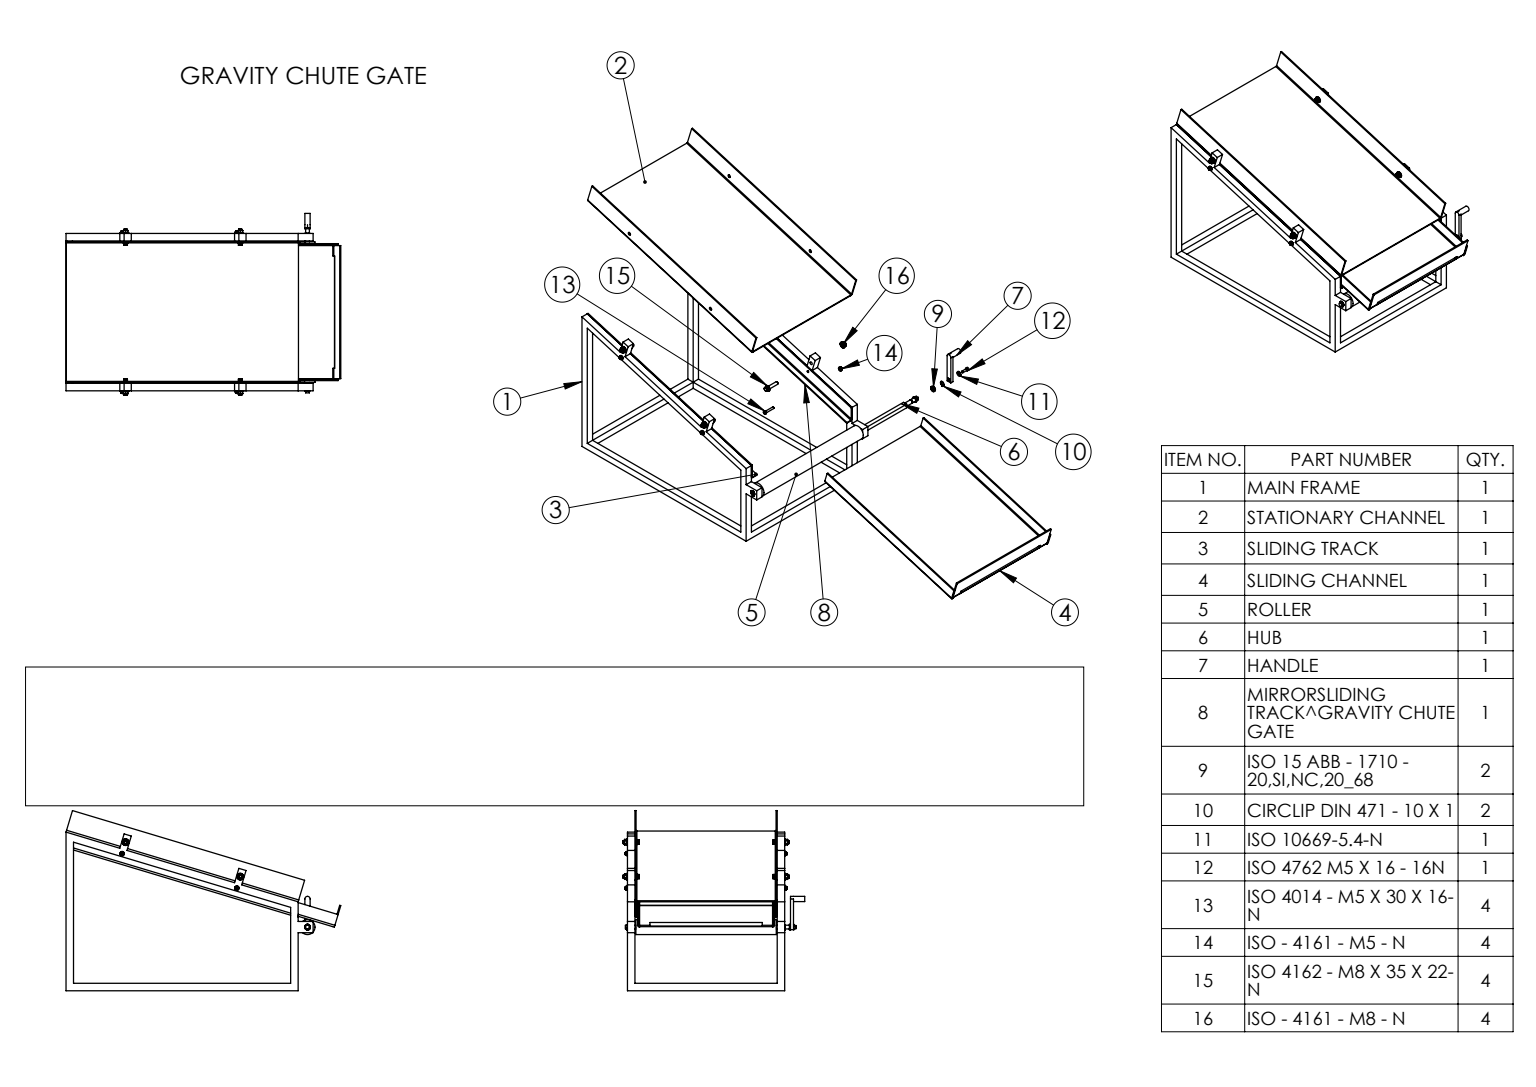
ISO-10303-21;
HEADER;
FILE_DESCRIPTION (('STEP AP214'),
    '1' );
FILE_NAME ('MAS-180',
    '2026-10-27T17:01:19',
    ( '' ),
    ( '' ),
    'SwSTEP 2.0',
    'SolidWorks 2026',
    '' );
FILE_SCHEMA (( 'AUTOMOTIVE_DESIGN' ));
ENDSEC;

DATA;
#1 = AXIS2_PLACEMENT_3D ( 'NONE', #9053, #14371, #13552 ) ;
#2 = DIRECTION ( 'NONE',  ( 1.000000000000000000, 0.000000000000000000, 0.000000000000000000 ) ) ;
#3 = ORIENTED_EDGE ( 'NONE', *, *, #2101, .F. ) ;
#4 = CIRCLE ( 'NONE', #4048, 4.799999999999999822 ) ;
#5 = ORIENTED_EDGE ( 'NONE', *, *, #10243, .F. ) ;
#6 = CARTESIAN_POINT ( 'NONE',  ( 1.058054217398695762, -6.894685612232789751, -0.3576316571898509600 ) ) ;
#7 = EDGE_CURVE ( 'NONE', #11993, #2660, #12348, .T. ) ;
#8 = FACE_OUTER_BOUND ( 'NONE', #13413, .T. ) ;
#9 = CIRCLE ( 'NONE', #4050, 0.7500000000000000000 ) ;
#10 = DIRECTION ( 'NONE',  ( 0.000000000000000000, 0.000000000000000000, -1.000000000000000000 ) ) ;
#11 = FACE_OUTER_BOUND ( 'NONE', #11887, .T. ) ;
#12 = ORIENTED_EDGE ( 'NONE', *, *, #9612, .F. ) ;
#13 =( GEOMETRIC_REPRESENTATION_CONTEXT ( 3 ) GLOBAL_UNCERTAINTY_ASSIGNED_CONTEXT ( ( #9752 ) ) GLOBAL_UNIT_ASSIGNED_CONTEXT ( ( #1212, #12871, #12805 ) ) REPRESENTATION_CONTEXT ( 'NONE', 'WORKASPACE' ) );
#14 = CARTESIAN_POINT ( 'NONE',  ( 640.0000000000000000, 160.0000000000000284, -222.5000000000000000 ) ) ;
#15 = EDGE_LOOP ( 'NONE', ( #6802, #6787, #9525 ) ) ;
#16 = ORIENTED_EDGE ( 'NONE', *, *, #2742, .F. ) ;
#17 = CARTESIAN_POINT ( 'NONE',  ( 6.212060063025091061, 2.039954613760103896, -5.000000000000000000 ) ) ;
#18 = EDGE_LOOP ( 'NONE', ( #9492, #7040, #7243, #2975 ) ) ;
#19 = TOROIDAL_SURFACE ( 'NONE', #6418, 2.700000000000000622, 0.2000000000000000111 ) ;
#20 = DIRECTION ( 'NONE',  ( 0.3420201433256622736, 1.150791560227853228E-16, 0.9396926207859106484 ) ) ;
#21 = CARTESIAN_POINT ( 'NONE',  ( 148.9991633467111569, 386.6211705227183870, -190.0000000000000000 ) ) ;
#22 = B_SPLINE_CURVE_WITH_KNOTS ( 'NONE', 3,
 ( #2566, #497, #13861, #11570, #12830, #4870, #11639, #4939 ),
 .UNSPECIFIED., .F., .F.,
 ( 4, 2, 2, 4 ),
 ( 0.002921158011986709890, 0.003648658599403064012, 0.004376159186819418567, 0.005831160361652128546 ),
 .UNSPECIFIED. ) ;
#23 = ORIENTED_EDGE ( 'NONE', *, *, #607, .T. ) ;
#24 = CARTESIAN_POINT ( 'NONE',  ( 6.244297270354683960, 1.800816419761795034E-11, 5.105276777067893512 ) ) ;
#25 = EDGE_CURVE ( 'NONE', #3163, #4002, #6451, .T. ) ;
#26 = DIRECTION ( 'NONE',  ( 0.000000000000000000, 0.000000000000000000, 1.000000000000000000 ) ) ;
#27 = FACE_OUTER_BOUND ( 'NONE', #636, .T. ) ;
#28 =( NAMED_UNIT ( * ) SI_UNIT ( $, .STERADIAN. ) SOLID_ANGLE_UNIT ( ) );
#29 = AXIS2_PLACEMENT_3D ( 'NONE', #668, #3321, #5190 ) ;
#30 = VERTEX_POINT ( 'NONE', #596 ) ;
#31 = EDGE_CURVE ( 'NONE', #4518, #4002, #1965, .T. ) ;
#32 = CARTESIAN_POINT ( 'NONE',  ( 0.000000000000000000, 0.000000000000000000, -25.03750572909317285 ) ) ;
#33 = ORIENTED_EDGE ( 'NONE', *, *, #12524, .T. ) ;
#34 = EDGE_CURVE ( 'NONE', #1936, #10044, #4903, .T. ) ;
#35 = AXIS2_PLACEMENT_3D ( 'NONE', #1338, #10342, #11594 ) ;
#36 = ORIENTED_EDGE ( 'NONE', *, *, #12069, .F. ) ;
#37 = CARTESIAN_POINT ( 'NONE',  ( 0.000000000000000000, 0.000000000000000000, -187.5000000000000000 ) ) ;
#38 = ADVANCED_FACE ( 'NONE', ( #6155 ), #1724, .F. ) ;
#39 = DIRECTION ( 'NONE',  ( 1.000000000000000000, 0.000000000000000000, 0.000000000000000000 ) ) ;
#40 = VECTOR ( 'NONE', #12593, 1000.000000000000000 ) ;
#41 = CARTESIAN_POINT ( 'NONE',  ( 164.3243839102495656, 402.9042173714779551, -210.0000000000000000 ) ) ;
#42 = CARTESIAN_POINT ( 'NONE',  ( 0.000000000000000000, 0.000000000000000000, 0.000000000000000000 ) ) ;
#43 = DIRECTION ( 'NONE',  ( 0.000000000000000000, 0.000000000000000000, -1.000000000000000000 ) ) ;
#44 = DIRECTION ( 'NONE',  ( 1.000000000000000000, 0.000000000000000000, -0.000000000000000000 ) ) ;
#45 = CARTESIAN_POINT ( 'NONE',  ( 702.5260191523640287, 164.1854586329053518, -177.6000000000005059 ) ) ;
#46 = ORIENTED_EDGE ( 'NONE', *, *, #6815, .F. ) ;
#47 = CYLINDRICAL_SURFACE ( 'NONE', #4191, 4.000000000000000000 ) ;
#48 = CARTESIAN_POINT ( 'NONE',  ( 6.527192678185238961, -5.883244248022514888, -3.079566767404799650E-14 ) ) ;
#49 = APPLICATION_PROTOCOL_DEFINITION ( 'draft international standard', 'automotive_design', 1998, #11586 ) ;
#50 = EDGE_LOOP ( 'NONE', ( #5774, #9979, #12011, #287 ) ) ;
#51=STYLED_ITEM('',(#14681),#12291);
#52 = ADVANCED_FACE ( 'NONE', ( #11739, #7114 ), #5117, .T. ) ;
#53 = CARTESIAN_POINT ( 'NONE',  ( 629.0000000000000000, 166.0000000000000284, -187.5000000000000000 ) ) ;
#54 = VERTEX_POINT ( 'NONE', #6074 ) ;
#55 = EDGE_LOOP ( 'NONE', ( #10980, #1481, #10748, #12698 ) ) ;
#56 = CARTESIAN_POINT ( 'NONE',  ( -20.63749999999999574, 0.000000000000000000, -6.975000000000000533 ) ) ;
#57 = CARTESIAN_POINT ( 'NONE',  ( -6.500000000000000000, 3.752776749732564809, -6.064240316920399110 ) ) ;
#58 = EDGE_CURVE ( 'NONE', #5396, #13410, #5058, .T. ) ;
#59 = FACE_OUTER_BOUND ( 'NONE', #3908, .T. ) ;
#60 = PLANE ( 'NONE',  #2621 ) ;
#61 = DIRECTION ( 'NONE',  ( 0.000000000000000000, 0.000000000000000000, 1.000000000000000000 ) ) ;
#62 = EDGE_LOOP ( 'NONE', ( #9424, #13653, #13087, #10601 ) ) ;
#63 = CARTESIAN_POINT ( 'NONE',  ( 6.244297270354684848, -1.799661607120071246E-11, -5.105276777067894400 ) ) ;
#64 = DIRECTION ( 'NONE',  ( 0.000000000000000000, 0.000000000000000000, 1.000000000000000000 ) ) ;
#65 = DIRECTION ( 'NONE',  ( 1.000000000000000000, 0.000000000000000000, 0.000000000000000000 ) ) ;
#66 = DIRECTION ( 'NONE',  ( 0.000000000000000000, 0.000000000000000000, 1.000000000000000000 ) ) ;
#67 = ORIENTED_EDGE ( 'NONE', *, *, #6101, .T. ) ;
#68 = ORIENTED_EDGE ( 'NONE', *, *, #2122, .F. ) ;
#69 = CARTESIAN_POINT ( 'NONE',  ( -3.511755186886750479, 2.826662030176366081, -3.597382984111578086 ) ) ;
#70 = PLANE ( 'NONE',  #7516 ) ;
#71 = CARTESIAN_POINT ( 'NONE',  ( -4.197393957002303999, 0.4069871074557429025, -3.503767560748926257 ) ) ;
#72 = VERTEX_POINT ( 'NONE', #2614 ) ;
#73 = B_SPLINE_CURVE_WITH_KNOTS ( 'NONE', 3,
 ( #5275, #111, #2574, #7961, #9298 ),
 .UNSPECIFIED., .F., .F.,
 ( 4, 1, 4 ),
 ( 0.000000000000000000, 0.002886751345948128985, 0.005773502691896257970 ),
 .UNSPECIFIED. ) ;
#74 = EDGE_LOOP ( 'NONE', ( #5773, #12707 ) ) ;
#75 = CARTESIAN_POINT ( 'NONE',  ( 609.6905198467529772, 186.4571330906553044, -187.4188186979287423 ) ) ;
#76 = CARTESIAN_POINT ( 'NONE',  ( 451.6722694765949768, 316.6998517015743460, -210.0000000000000000 ) ) ;
#77 = EDGE_CURVE ( 'NONE', #2441, #3014, #1734, .T. ) ;
#78 = DIRECTION ( 'NONE',  ( 0.000000000000000000, 0.000000000000000000, -1.000000000000000000 ) ) ;
#79 = CARTESIAN_POINT ( 'NONE',  ( 650.0000000000000000, 175.0000000000000568, 190.0000000000000000 ) ) ;
#80 = CARTESIAN_POINT ( 'NONE',  ( 459.7035746174795463, 294.6698471414878782, 210.0000000000000000 ) ) ;
#81 = ORIENTED_EDGE ( 'NONE', *, *, #14582, .T. ) ;
#82 = DIRECTION ( 'NONE',  ( 1.000000000000000000, 0.000000000000000000, 0.000000000000000000 ) ) ;
#83 = ORIENTED_EDGE ( 'NONE', *, *, #7565, .F. ) ;
#84 = ORIENTED_EDGE ( 'NONE', *, *, #4575, .F. ) ;
#85 = CARTESIAN_POINT ( 'NONE',  ( 642.5000000000001137, 160.0000000000000284, -207.0000000000000000 ) ) ;
#86 = ORIENTED_EDGE ( 'NONE', *, *, #13517, .T. ) ;
#87 = ADVANCED_FACE ( 'NONE', ( #9552, #4013, #2686 ), #14052, .T. ) ;
#88 = EDGE_CURVE ( 'NONE', #5056, #3419, #11622, .T. ) ;
#89 = CARTESIAN_POINT ( 'NONE',  ( 0.000000000000000000, 0.000000000000000000, -7.381345277524544279 ) ) ;
#90 = DIRECTION ( 'NONE',  ( 1.000000000000000000, 0.000000000000000000, 0.000000000000000000 ) ) ;
#91 = ORIENTED_EDGE ( 'NONE', *, *, #14281, .F. ) ;
#92 = CARTESIAN_POINT ( 'NONE',  ( 2.500000000000000888, 3.061616997868384127E-16, -4.974599999999998801 ) ) ;
#93 = DIRECTION ( 'NONE',  ( 0.9578262852211525402, -0.2873478855663419429, -0.000000000000000000 ) ) ;
#94 = DIRECTION ( 'NONE',  ( 1.000000000000000000, 0.000000000000000000, 0.000000000000000000 ) ) ;
#95 = SURFACE_STYLE_USAGE ( .BOTH. , #11266 ) ;
#96 = SHAPE_REPRESENTATION_RELATIONSHIP ( 'NONE' , 'NONE' ,  #14430, #6538 ) ;
#97 = ORIENTED_EDGE ( 'NONE', *, *, #10462, .F. ) ;
#98 = PLANE ( 'NONE',  #9893 ) ;
#99 = EDGE_LOOP ( 'NONE', ( #7071, #6114, #7487, #2779 ) ) ;
#100 = EDGE_LOOP ( 'NONE', ( #955, #2493 ) ) ;
#101 = DIRECTION ( 'NONE',  ( 0.000000000000000000, 0.000000000000000000, 1.000000000000000000 ) ) ;
#102 = ADVANCED_FACE ( 'NONE', ( #9327 ), #3935, .F. ) ;
#103 = CARTESIAN_POINT ( 'NONE',  ( 642.4999005938085475, 159.0059381730093548, -210.0000000000000284 ) ) ;
#104 = CARTESIAN_POINT ( 'NONE',  ( 642.5000000000001137, 160.0000000000000284, 210.0000119999999981 ) ) ;
#105 = LINE ( 'NONE', #11206, #8037 ) ;
#106 = EDGE_CURVE ( 'NONE', #2067, #2328, #1941, .T. ) ;
#107 = CARTESIAN_POINT ( 'NONE',  ( 0.3572655899081578768, -4.618802153516999631, -3.329030144205522754E-16 ) ) ;
#108 = CARTESIAN_POINT ( 'NONE',  ( 610.0000000000000000, 227.4403065089097993, 184.7999999999999829 ) ) ;
#109 = DIRECTION ( 'NONE',  ( 0.000000000000000000, 0.000000000000000000, 1.000000000000000000 ) ) ;
#110 = EDGE_LOOP ( 'NONE', ( #11251, #9027, #7663, #8176 ) ) ;
#111 = CARTESIAN_POINT ( 'NONE',  ( 6.196878017913832970, -3.367876570272823500, -4.166666666666666963 ) ) ;
#112 = CARTESIAN_POINT ( 'NONE',  ( 0.000000000000000000, 0.000000000000000000, -4.974599999999998801 ) ) ;
#113 = CARTESIAN_POINT ( 'NONE',  ( 6.403457969954073015, -5.776886471390939803, 5.182398524903814613E-16 ) ) ;
#114 = CONTEXT_DEPENDENT_SHAPE_REPRESENTATION ( #6028, #6295 ) ;
#115 = ORIENTED_EDGE ( 'NONE', *, *, #8446, .T. ) ;
#116 = CARTESIAN_POINT ( 'NONE',  ( 145.1678582058265476, 408.6511750828048548, -190.0000000000000000 ) ) ;
#117 = ORIENTED_EDGE ( 'NONE', *, *, #9862, .T. ) ;
#118 = ORIENTED_EDGE ( 'NONE', *, *, #8596, .T. ) ;
#119 = SURFACE_STYLE_USAGE ( .BOTH. , #3632 ) ;
#120 = DIRECTION ( 'NONE',  ( -1.673149720584257832E-16, 4.625616335171366110E-15, 1.000000000000000000 ) ) ;
#121 = EDGE_CURVE ( 'NONE', #14270, #6163, #532, .T. ) ;
#122 = CARTESIAN_POINT ( 'NONE',  ( 6.534838248920896930, -2.951765777552407766, 5.112608298763836601 ) ) ;
#123 = EDGE_CURVE ( 'NONE', #7138, #2816, #1501, .T. ) ;
#124 = PRODUCT ( 'plain washer 10669 type nl_iso_ISO 10669-5.4-N', 'plain washer 10669 type nl_iso_ISO 10669-5.4-N', '', ( #6717 ) ) ;
#125 = CARTESIAN_POINT ( 'NONE',  ( 716.7018481736364492, 193.3416907550361827, -179.8000000000001535 ) ) ;
#126 = EDGE_CURVE ( 'NONE', #13510, #3531, #3853, .T. ) ;
#127 = UNCERTAINTY_MEASURE_WITH_UNIT (LENGTH_MEASURE( 1.000000000000000082E-05 ), #3308, 'distance_accuracy_value', 'NONE');
#128 = CARTESIAN_POINT ( 'NONE',  ( 630.0000000000000000, 160.0000000000000284, 215.5000000000000000 ) ) ;
#129 = ORIENTED_EDGE ( 'NONE', *, *, #11764, .F. ) ;
#130 = EDGE_CURVE ( 'NONE', #2847, #2989, #365, .T. ) ;
#131 = DIRECTION ( 'NONE',  ( 0.000000000000000000, 0.000000000000000000, 1.000000000000000000 ) ) ;
#132 = CARTESIAN_POINT ( 'NONE',  ( 610.0000000000000000, 0.000000000000000000, -210.0000000000000000 ) ) ;
#133 = SURFACE_STYLE_FILL_AREA ( #3350 ) ;
#134 = CARTESIAN_POINT ( 'NONE',  ( 650.0000000000000000, 0.000000000000000000, 0.000000000000000000 ) ) ;
#135 = ORIENTED_EDGE ( 'NONE', *, *, #9646, .T. ) ;
#136 = ORIENTED_EDGE ( 'NONE', *, *, #1223, .F. ) ;
#137 = CARTESIAN_POINT ( 'NONE',  ( 641.5533979126569193, 156.2228576472182624, 210.0000119999999981 ) ) ;
#138 = DIRECTION ( 'NONE',  ( -1.000000000000000000, 0.000000000000000000, 0.000000000000000000 ) ) ;
#139 = LINE ( 'NONE', #7921, #12453 ) ;
#140 = CARTESIAN_POINT ( 'NONE',  ( 9.498873539028489220E-16, -10.00000000000000000, 210.0000000000000000 ) ) ;
#141 = EDGE_CURVE ( 'NONE', #2225, #13547, #11826, .T. ) ;
#143 = ORIENTED_EDGE ( 'NONE', *, *, #1858, .T. ) ;
#142 = CIRCLE ( 'NONE', #4214, 5.000000000000004441 ) ;
#144 = VECTOR ( 'NONE', #10565, 1000.000000000000000 ) ;
#145 = VERTEX_POINT ( 'NONE', #14118 ) ;
#146 = DIRECTION ( 'NONE',  ( 0.000000000000000000, 0.000000000000000000, -1.000000000000000000 ) ) ;
#147 = DIRECTION ( 'NONE',  ( 0.000000000000000000, 0.000000000000000000, 1.000000000000000000 ) ) ;
#148 = FACE_BOUND ( 'NONE', #8389, .T. ) ;
#149 = DIRECTION ( 'NONE',  ( 0.000000000000000000, 1.000000000000000000, -4.159212477520619976E-15 ) ) ;
#150 = CARTESIAN_POINT ( 'NONE',  ( 142.4540310085880606, 355.9707293956415697, 187.0000000000000000 ) ) ;
#151 = VERTEX_POINT ( 'NONE', #13018 ) ;
#152 = CYLINDRICAL_SURFACE ( 'NONE', #12239, 4.000000000000000000 ) ;
#153 = EDGE_LOOP ( 'NONE', ( #10187, #6954 ) ) ;
#154 = ORIENTED_EDGE ( 'NONE', *, *, #12359, .F. ) ;
#155 = CARTESIAN_POINT ( 'NONE',  ( -6.259644161404860030E-16, -4.618802153517027165, -5.000000000000000000 ) ) ;
#156 = VECTOR ( 'NONE', #9588, 1000.000000000000000 ) ;
#157 = EDGE_CURVE ( 'NONE', #12209, #11318, #10435, .T. ) ;
#158 = VECTOR ( 'NONE', #9040, 1000.000000000000000 ) ;
#159 = PRODUCT_DEFINITION_SHAPE ( 'NONE', 'NONE',  #14640 ) ;
#160 = ADVANCED_FACE ( 'NONE', ( #9907 ), #3261, .F. ) ;
#161 = CARTESIAN_POINT ( 'NONE',  ( 112.3905262037967248, 374.6350873459896320, 182.7999999999994714 ) ) ;
#162 =( REPRESENTATION_RELATIONSHIP ('NONE','NONE', #2822, #5462 ) REPRESENTATION_RELATIONSHIP_WITH_TRANSFORMATION ( #13326 )SHAPE_REPRESENTATION_RELATIONSHIP( ) );
#163 = DIRECTION ( 'NONE',  ( 1.000000000000000000, 0.000000000000000000, 0.000000000000000000 ) ) ;
#164 = ORIENTED_EDGE ( 'NONE', *, *, #10968, .F. ) ;
#165 = CARTESIAN_POINT ( 'NONE',  ( 459.3348797583642522, 272.6398425814014104, -210.0000000000000000 ) ) ;
#166 = FACE_OUTER_BOUND ( 'NONE', #2918, .T. ) ;
#167 = AXIS2_PLACEMENT_3D ( 'NONE', #3930, #8417, #10718 ) ;
#168 = AXIS2_PLACEMENT_3D ( 'NONE', #10064, #3978, #5431 ) ;
#169 = CARTESIAN_POINT ( 'NONE',  ( 1.500000000000001332, 0.000000000000000000, 0.000000000000000000 ) ) ;
#170 = CARTESIAN_POINT ( 'NONE',  ( 0.6507732100473444525, -4.243078065514795050, -0.2236248678334952777 ) ) ;
#171 = ORIENTED_EDGE ( 'NONE', *, *, #13700, .T. ) ;
#172 = DIRECTION ( 'NONE',  ( 3.340694023494469140E-16, -4.069768234201303760E-15, -1.000000000000000000 ) ) ;
#173 = VERTEX_POINT ( 'NONE', #3127 ) ;
#174 = ORIENTED_EDGE ( 'NONE', *, *, #7655, .T. ) ;
#175 = LINE ( 'NONE', #4721, #7503 ) ;
#176 = VECTOR ( 'NONE', #3313, 1000.000000000000000 ) ;
#177 = MECHANICAL_DESIGN_GEOMETRIC_PRESENTATION_REPRESENTATION (  '', ( #1004 ), #8687 ) ;
#178 = DIRECTION ( 'NONE',  ( 0.000000000000000000, 0.000000000000000000, -1.000000000000000000 ) ) ;
#179 = DIRECTION ( 'NONE',  ( -1.000000000000000000, -0.000000000000000000, -0.000000000000000000 ) ) ;
#180 = ORIENTED_EDGE ( 'NONE', *, *, #12151, .F. ) ;
#181 = DIRECTION ( 'NONE',  ( 1.000000000000000000, 0.000000000000000000, 0.000000000000000000 ) ) ;
#182 = CIRCLE ( 'NONE', #10114, 0.2000000000000000944 ) ;
#183 = CARTESIAN_POINT ( 'NONE',  ( 610.0421465541240877, 190.7920056415575516, -186.9999999999999432 ) ) ;
#184 = CARTESIAN_POINT ( 'NONE',  ( -6.826425371444817536, 2.641426549045769345, -6.344843397090116355 ) ) ;
#185 = PLANE ( 'NONE',  #4357 ) ;
#186 = EDGE_CURVE ( 'NONE', #3815, #10556, #4083, .T. ) ;
#187 = ORIENTED_EDGE ( 'NONE', *, *, #791, .F. ) ;
#188 = VECTOR ( 'NONE', #2606, 1000.000000000000000 ) ;
#189 = AXIS2_PLACEMENT_3D ( 'NONE', #8607, #13111, #14291 ) ;
#190 = FACE_OUTER_BOUND ( 'NONE', #11579, .T. ) ;
#191 = DIRECTION ( 'NONE',  ( 1.000000000000000000, 0.000000000000000000, 0.000000000000000000 ) ) ;
#192 = LINE ( 'NONE', #8454, #3753 ) ;
#193 = EDGE_LOOP ( 'NONE', ( #2834, #237, #12964, #6241 ) ) ;
#194 = VECTOR ( 'NONE', #6776, 1000.000000000000000 ) ;
#195 = CARTESIAN_POINT ( 'NONE',  ( 6.327640840229819652, -2.033197012992983943, 4.999999999998298250 ) ) ;
#196 = ORIENTED_EDGE ( 'NONE', *, *, #8935, .F. ) ;
#197 = VERTEX_POINT ( 'NONE', #7549 ) ;
#198 = DIRECTION ( 'NONE',  ( -1.000000000000000000, 0.000000000000000000, 0.000000000000000000 ) ) ;
#199 = CARTESIAN_POINT ( 'NONE',  ( 726.1975094929949819, 167.5243180396262801, -149.9999999999986358 ) ) ;
#200 = VECTOR ( 'NONE', #9426, 1000.000000000000000 ) ;
#201 = CARTESIAN_POINT ( 'NONE',  ( 0.000000000000000000, 0.000000000000000000, 6.250000000000000000 ) ) ;
#202 = VECTOR ( 'NONE', #5695, 1000.000000000000000 ) ;
#203 = AXIS2_PLACEMENT_3D ( 'NONE', #4127, #790, #8616 ) ;
#204 = CARTESIAN_POINT ( 'NONE',  ( 6.269955739554010421, 4.268932597852939104, -6.443844059477442876 ) ) ;
#205 = LINE ( 'NONE', #12625, #7486 ) ;
#206 = ADVANCED_FACE ( 'NONE', ( #6452 ), #11002, .F. ) ;
#207 = ORIENTED_EDGE ( 'NONE', *, *, #12524, .F. ) ;
#208 = CIRCLE ( 'NONE', #11778, 8.542937654374687995 ) ;
#209 = FACE_OUTER_BOUND ( 'NONE', #12548, .T. ) ;
#210 = DIRECTION ( 'NONE',  ( 0.000000000000000000, 0.000000000000000000, 1.000000000000000000 ) ) ;
#211 = EDGE_CURVE ( 'NONE', #1708, #13374, #7694, .T. ) ;
#212 = VECTOR ( 'NONE', #12362, 1000.000000000000000 ) ;
#213 = DIRECTION ( 'NONE',  ( 0.000000000000000000, -0.000000000000000000, -1.000000000000000000 ) ) ;
#214 = VERTEX_POINT ( 'NONE', #14200 ) ;
#215 = ORIENTED_EDGE ( 'NONE', *, *, #1697, .T. ) ;
#216 = CARTESIAN_POINT ( 'NONE',  ( 640.9975013179864618, 155.3908996001881064, 210.0000119999999981 ) ) ;
#217 = CARTESIAN_POINT ( 'NONE',  ( 145.1678582058265192, 408.6511750828049117, 210.0000000000000000 ) ) ;
#218 = EDGE_CURVE ( 'NONE', #4236, #7201, #9506, .T. ) ;
#219 = CARTESIAN_POINT ( 'NONE',  ( 6.390820841722129941, 2.823237767533145703, 5.110008744785254464 ) ) ;
#220 = CIRCLE ( 'NONE', #10375, 2.199999999999988187 ) ;
#221 = AXIS2_PLACEMENT_3D ( 'NONE', #1029, #9011, #10110 ) ;
#222 = EDGE_CURVE ( 'NONE', #5688, #13812, #7865, .T. ) ;
#223 = CIRCLE ( 'NONE', #9439, 5.000000000000000000 ) ;
#224 = ORIENTED_EDGE ( 'NONE', *, *, #3254, .F. ) ;
#225 = VECTOR ( 'NONE', #9137, 1000.000000000000114 ) ;
#226 = ORIENTED_EDGE ( 'NONE', *, *, #14281, .T. ) ;
#227 = DIRECTION ( 'NONE',  ( 0.000000000000000000, 0.000000000000000000, -1.000000000000000000 ) ) ;
#228 = CARTESIAN_POINT ( 'NONE',  ( 2.263183130831067924, -6.566419505188284766, -6.208110906918261840 ) ) ;
#229 = LINE ( 'NONE', #12418, #8916 ) ;
#230 = DIRECTION ( 'NONE',  ( -1.000000000000000000, 0.000000000000000000, 0.000000000000000000 ) ) ;
#231 = CARTESIAN_POINT ( 'NONE',  ( 635.0000000000000000, 160.0000000000000284, 215.5000000000000000 ) ) ;
#232 = SURFACE_SIDE_STYLE ('',( #9558 ) ) ;
#233 = VECTOR ( 'NONE', #11079, 1000.000000000000000 ) ;
#234 = ORIENTED_EDGE ( 'NONE', *, *, #11746, .T. ) ;
#235 = AXIS2_PLACEMENT_3D ( 'NONE', #506, #13872, #10410 ) ;
#236 = DIRECTION ( 'NONE',  ( 0.000000000000000000, 0.000000000000000000, 1.000000000000000000 ) ) ;
#237 = ORIENTED_EDGE ( 'NONE', *, *, #8274, .T. ) ;
#238 = VERTEX_POINT ( 'NONE', #752 ) ;
#239 = LINE ( 'NONE', #9271, #6395 ) ;
#240 = EDGE_CURVE ( 'NONE', #4614, #6705, #3374, .T. ) ;
#241 = VECTOR ( 'NONE', #10180, 1000.000000000000000 ) ;
#242 = EDGE_CURVE ( 'NONE', #7278, #11617, #2972, .T. ) ;
#243 = ADVANCED_FACE ( 'NONE', ( #12113 ), #8583, .F. ) ;
#244 = DIRECTION ( 'NONE',  ( 0.9578262852211513190, -0.2873478855663453846, 0.000000000000000000 ) ) ;
#245 = CIRCLE ( 'NONE', #8768, 4.199999999999926459 ) ;
#246 = AXIS2_PLACEMENT_3D ( 'NONE', #1497, #5996, #10494 ) ;
#247 = LINE ( 'NONE', #13705, #494 ) ;
#248 = VERTEX_POINT ( 'NONE', #7468 ) ;
#249 = DIRECTION ( 'NONE',  ( 0.9578262852211507639, -0.2873478855663477716, 0.000000000000000000 ) ) ;
#250 = CARTESIAN_POINT ( 'NONE',  ( 153.1991633467111456, 386.6211705227183870, -210.0000000000000000 ) ) ;
#251 = CARTESIAN_POINT ( 'NONE',  ( 627.2408731339806991, 284.9098836221797342, 190.0000000000001990 ) ) ;
#252 = PLANE ( 'NONE',  #3852 ) ;
#253 = ORIENTED_EDGE ( 'NONE', *, *, #3737, .F. ) ;
#254 = CARTESIAN_POINT ( 'NONE',  ( 10.00000000000000000, 0.000000000000000000, 210.0000000000000000 ) ) ;
#255 = ORIENTED_EDGE ( 'NONE', *, *, #504, .F. ) ;
#256 = VECTOR ( 'NONE', #3741, 1000.000000000000000 ) ;
#257 = ORIENTED_EDGE ( 'NONE', *, *, #4905, .T. ) ;
#258 = CARTESIAN_POINT ( 'NONE',  ( 10.00000000000000000, 386.5596934910894902, -190.0000000000000000 ) ) ;
#259 = COLOUR_RGB ( '',1.000000000000000000, 0.9490196078431372140, 0.9098039215686274384 ) ;
#260 =( BOUNDED_SURFACE ( )  B_SPLINE_SURFACE ( 3, 2, ( 
 ( #2546, #4855, #7134 ),
 ( #13843, #1521, #11762 ),
 ( #3742, #1668, #2637 ),
 ( #552, #8754, #12960 ),
 ( #1882, #8671, #14357 ),
 ( #14286, #6532, #7425 ),
 ( #11025, #772, #8601 ),
 ( #4037, #14440, #13175 ) ),
 .UNSPECIFIED., .F., .F., .F. ) 
 B_SPLINE_SURFACE_WITH_KNOTS ( ( 4, 2, 2, 4 ),
 ( 3, 3 ),
 ( 0.03170918191602133812, 0.03570420671717101924, 0.03770171911774586326, 0.03969923151832070729 ),
 ( 0.000000000000000000, 1.000000000000000000 ),
 .UNSPECIFIED. ) 
 GEOMETRIC_REPRESENTATION_ITEM ( )  RATIONAL_B_SPLINE_SURFACE ( (
 ( 1.000000000000000000, 0.8047781070930550840, 1.000000000000000000),
 ( 1.000000000000000000, 0.8123787894255611874, 1.000000000000000000),
 ( 1.000000000000000000, 0.8190667557154468481, 1.000000000000000000),
 ( 1.000000000000000000, 0.8191933945820784047, 1.000000000000000000),
 ( 1.000000000000000000, 0.8176087340369108114, 1.000000000000000000),
 ( 1.000000000000000000, 0.8122956952719621038, 1.000000000000000000),
 ( 1.000000000000000000, 0.8086308540103167575, 1.000000000000000000),
 ( 1.000000000000000000, 0.8047712493762134711, 1.000000000000000000) ) ) 
 REPRESENTATION_ITEM ( '' )  SURFACE ( )  );
#261 = LINE ( 'NONE', #1530, #10839 ) ;
#262 = DIRECTION ( 'NONE',  ( -0.000000000000000000, -0.000000000000000000, -1.000000000000000000 ) ) ;
#263 = VECTOR ( 'NONE', #2526, 1000.000000000000000 ) ;
#264 = VERTEX_POINT ( 'NONE', #11962 ) ;
#265 = CARTESIAN_POINT ( 'NONE',  ( 459.7035746174795463, 294.6698471414878782, -210.0000000000000000 ) ) ;
#266 = FACE_OUTER_BOUND ( 'NONE', #13109, .T. ) ;
#267 = CARTESIAN_POINT ( 'NONE',  ( 635.0000000000000000, 160.0000000000000284, 211.0000000000000000 ) ) ;
#268 = CARTESIAN_POINT ( 'NONE',  ( 610.0000000000001137, 185.6790804732684137, 184.8000000000000682 ) ) ;
#269 = ORIENTED_EDGE ( 'NONE', *, *, #1906, .F. ) ;
#270 = PRODUCT_DEFINITION_FORMATION_WITH_SPECIFIED_SOURCE ( 'ANY', '', #8554, .NOT_KNOWN. ) ;
#271 = CARTESIAN_POINT ( 'NONE',  ( 21.00000000000000355, 0.000000000000000000, 0.000000000000000000 ) ) ;
#272 = CARTESIAN_POINT ( 'NONE',  ( 6.355827204229361982, 5.411702751981842141, -0.8440485055075606091 ) ) ;
#273 = CONTEXT_DEPENDENT_SHAPE_REPRESENTATION ( #1310, #11832 ) ;
#274 = ORIENTED_EDGE ( 'NONE', *, *, #3153, .F. ) ;
#275 = CARTESIAN_POINT ( 'NONE',  ( 0.000000000000000000, 0.000000000000000000, 0.000000000000000000 ) ) ;
#276 = ORIENTED_EDGE ( 'NONE', *, *, #2072, .F. ) ;
#277 = EDGE_LOOP ( 'NONE', ( #11682, #4913 ) ) ;
#278 = CARTESIAN_POINT ( 'NONE',  ( 4.000000000000000000, -2.309401076758514915, -3.433295621305383349 ) ) ;
#279 = CYLINDRICAL_SURFACE ( 'NONE', #8252, 4.799999999999999822 ) ;
#280 = LINE ( 'NONE', #3777, #11997 ) ;
#281 = EDGE_CURVE ( 'NONE', #5961, #525, #3049, .T. ) ;
#282 = ADVANCED_FACE ( 'NONE', ( #6369 ), #14593, .F. ) ;
#283 = CARTESIAN_POINT ( 'NONE',  ( 112.9652219749295341, 376.5507399164317803, -190.0000000000000000 ) ) ;
#284 = UNCERTAINTY_MEASURE_WITH_UNIT (LENGTH_MEASURE( 1.000000000000000082E-05 ), #8450, 'distance_accuracy_value', 'NONE');
#285 = VECTOR ( 'NONE', #13609, 1000.000000000000000 ) ;
#286 = LINE ( 'NONE', #5042, #1068 ) ;
#287 = ORIENTED_EDGE ( 'NONE', *, *, #8174, .T. ) ;
#288 = DIRECTION ( 'NONE',  ( -0.2873478855663281206, -0.9578262852211566480, -1.261617073437843370E-13 ) ) ;
#289 = LINE ( 'NONE', #6055, #6795 ) ;
#290 = DIRECTION ( 'NONE',  ( 1.000000000000000000, 0.000000000000000000, 0.000000000000000000 ) ) ;
#291 = LINE ( 'NONE', #8346, #11794 ) ;
#292 = ORIENTED_EDGE ( 'NONE', *, *, #6303, .T. ) ;
#293 = VERTEX_POINT ( 'NONE', #4374 ) ;
#294 = FACE_OUTER_BOUND ( 'NONE', #6811, .T. ) ;
#295 = CARTESIAN_POINT ( 'NONE',  ( 3.500000000000000000, 2.309401076758500704, -4.000000000000000000 ) ) ;
#296 = CARTESIAN_POINT ( 'NONE',  ( 6.095473853218515536, 3.806361898857873793, 3.407187799183811983 ) ) ;
#297 = EDGE_CURVE ( 'NONE', #14514, #7459, #997, .T. ) ;
#298 = ORIENTED_EDGE ( 'NONE', *, *, #11153, .T. ) ;
#299 = VERTEX_POINT ( 'NONE', #5768 ) ;
#300 = CARTESIAN_POINT ( 'NONE',  ( 650.0000000000000000, 175.0000000000000568, 210.0000000000000000 ) ) ;
#301 = FACE_OUTER_BOUND ( 'NONE', #4804, .T. ) ;
#302 = EDGE_CURVE ( 'NONE', #2242, #4648, #7848, .T. ) ;
#303 = CARTESIAN_POINT ( 'NONE',  ( 6.466260427357664931, 5.808561367196023006, 9.218349649774728207E-16 ) ) ;
#304 = DIRECTION ( 'NONE',  ( 0.2873478855663427756, 0.9578262852211522071, 3.408579461568464094E-15 ) ) ;
#305 = DIRECTION ( 'NONE',  ( 1.000000000000000000, 0.000000000000000000, 0.000000000000000000 ) ) ;
#306 = ORIENTED_EDGE ( 'NONE', *, *, #7465, .F. ) ;
#307 = CARTESIAN_POINT ( 'NONE',  ( -0.1404048886732797152, -4.699864953788083888, -3.686887068327043160 ) ) ;
#308 = ORIENTED_EDGE ( 'NONE', *, *, #14248, .F. ) ;
#309 = EDGE_LOOP ( 'NONE', ( #11418, #2643 ) ) ;
#310 = CARTESIAN_POINT ( 'NONE',  ( 229.2257385731833779, 308.4724102386176128, -177.6000000000002217 ) ) ;
#311 = EDGE_CURVE ( 'NONE', #1794, #10356, #7010, .T. ) ;
#312 = CARTESIAN_POINT ( 'NONE',  ( 2.500000000000000000, 0.000000000000000000, 2.041999999999999815 ) ) ;
#313 = LINE ( 'NONE', #2471, #1913 ) ;
#314 = LINE ( 'NONE', #3891, #1590 ) ;
#315 = ORIENTED_EDGE ( 'NONE', *, *, #8291, .F. ) ;
#316 = CARTESIAN_POINT ( 'NONE',  ( 1.391697335622810172, 4.043246145443375461, -3.503898532754365913 ) ) ;
#317 = FACE_OUTER_BOUND ( 'NONE', #9908, .T. ) ;
#318 = ADVANCED_FACE ( 'NONE', ( #7912 ), #1489, .F. ) ;
#319 = DIRECTION ( 'NONE',  ( 0.000000000000000000, 0.000000000000000000, 1.000000000000000000 ) ) ;
#320 = CARTESIAN_POINT ( 'NONE',  ( 440.1783540539412343, 278.3868002927283101, -190.0000000000000000 ) ) ;
#321 = EDGE_LOOP ( 'NONE', ( #9410, #8500, #10695 ) ) ;
#322 = EDGE_CURVE ( 'NONE', #11174, #11494, #10043, .T. ) ;
#323 = CARTESIAN_POINT ( 'NONE',  ( -8.505790995054899994, 376.6597771564184427, -184.8000000000000398 ) ) ;
#324 = VECTOR ( 'NONE', #11210, 1000.000000000000000 ) ;
#325 = PRODUCT_RELATED_PRODUCT_CATEGORY ( 'part', '', ( #2905 ) ) ;
#326 = ORIENTED_EDGE ( 'NONE', *, *, #6236, .F. ) ;
#327 = ORIENTED_EDGE ( 'NONE', *, *, #242, .F. ) ;
#328 = CARTESIAN_POINT ( 'NONE',  ( -0.1481481481481481122, -4.797713218419819903, -1.000000000000000000 ) ) ;
#329 = CIRCLE ( 'NONE', #7673, 4.000000000000000000 ) ;
#330 = CARTESIAN_POINT ( 'NONE',  ( -20.63749999999999574, 0.000000000000000000, 0.000000000000000000 ) ) ;
#331 = LINE ( 'NONE', #7064, #10396 ) ;
#332 = ORIENTED_EDGE ( 'NONE', *, *, #5036, .F. ) ;
#333 = CARTESIAN_POINT ( 'NONE',  ( 609.8668404561643683, 185.6877074168924935, 185.4847245573741930 ) ) ;
#334 = DIRECTION ( 'NONE',  ( 1.501925087425806625E-16, 4.055197736049677764E-15, 1.000000000000000000 ) ) ;
#335 = DIRECTION ( 'NONE',  ( -1.000000000000000000, -0.000000000000000000, -0.000000000000000000 ) ) ;
#336 = CARTESIAN_POINT ( 'NONE',  ( 145.1678582058265192, 408.6511750828049117, 210.0000000000000000 ) ) ;
#337 = ORIENTED_EDGE ( 'NONE', *, *, #5739, .T. ) ;
#338 = FACE_OUTER_BOUND ( 'NONE', #7888, .T. ) ;
#339 = SURFACE_STYLE_FILL_AREA ( #5976 ) ;
#340 = ORIENTED_EDGE ( 'NONE', *, *, #7667, .F. ) ;
#341 = CARTESIAN_POINT ( 'NONE',  ( 6.207541730803228575, -1.039448978216581665, 5.000000000000000888 ) ) ;
#342 = SHAPE_REPRESENTATION ( 'Mirrorsliding track^MAS-180', ( #9440 ), #8524 ) ;
#343 = ORIENTED_EDGE ( 'NONE', *, *, #2161, .T. ) ;
#344 = VERTEX_POINT ( 'NONE', #128 ) ;
#345 =( NAMED_UNIT ( * ) SI_UNIT ( $, .STERADIAN. ) SOLID_ANGLE_UNIT ( ) );
#346 = CARTESIAN_POINT ( 'NONE',  ( 0.1391502195351337900, -4.241015250120798719, 0.6543461111163306754 ) ) ;
#347 = EDGE_CURVE ( 'NONE', #8605, #12947, #205, .T. ) ;
#348 = CARTESIAN_POINT ( 'NONE',  ( 6.367873360227555679, -2.886751345948120662, 4.999999999999999112 ) ) ;
#349 = EDGE_CURVE ( 'NONE', #6917, #2433, #2048, .T. ) ;
#350 = CARTESIAN_POINT ( 'NONE',  ( -31.74999999999995737, 0.000000000000000000, 0.000000000000000000 ) ) ;
#351 = DIRECTION ( 'NONE',  ( 1.000000000000000000, 0.000000000000000000, 0.000000000000000000 ) ) ;
#352 = VERTEX_POINT ( 'NONE', #14549 ) ;
#353 = CARTESIAN_POINT ( 'NONE',  ( -3.836423976351538233E-15, 4.452621892014634319, 2.287832656137188447 ) ) ;
#354 = DIRECTION ( 'NONE',  ( -0.000000000000000000, 0.5000000000000014433, 0.8660254037844378194 ) ) ;
#355 = DIRECTION ( 'NONE',  ( 0.000000000000000000, 0.000000000000000000, 1.000000000000000000 ) ) ;
#356 = CARTESIAN_POINT ( 'NONE',  ( 6.495567275914603478, 2.917443832165053763, 5.053160945538326843 ) ) ;
#357 = EDGE_CURVE ( 'NONE', #9335, #3684, #13663, .T. ) ;
#358 = VERTEX_POINT ( 'NONE', #9242 ) ;
#359 = EDGE_LOOP ( 'NONE', ( #3831, #5633, #326, #12007 ) ) ;
#360 = CARTESIAN_POINT ( 'NONE',  ( 6.815830331203684089, -0.6610623347507956771, -6.171384342982605631 ) ) ;
#361 = DIRECTION ( 'NONE',  ( -1.000000000000000000, 0.000000000000000000, 0.000000000000000000 ) ) ;
#362 = DIRECTION ( 'NONE',  ( -0.8191520442889902442, 0.000000000000000000, -0.5735764363510482688 ) ) ;
#363 = ORIENTED_EDGE ( 'NONE', *, *, #918, .F. ) ;
#364 = ADVANCED_FACE ( 'NONE', ( #9021 ), #12395, .F. ) ;
#365 = LINE ( 'NONE', #2825, #10917 ) ;
#366 = CARTESIAN_POINT ( 'NONE',  ( 610.6379424248335681, 188.7103817868187150, -185.3679143846944157 ) ) ;
#367 = DIRECTION ( 'NONE',  ( -1.102263794767363534E-15, -3.674212649225433764E-15, -1.000000000000000000 ) ) ;
#368 = DIRECTION ( 'NONE',  ( -0.000000000000000000, -0.000000000000000000, 1.000000000000000000 ) ) ;
#369 = DIRECTION ( 'NONE',  ( 0.000000000000000000, 0.000000000000000000, -1.000000000000000000 ) ) ;
#370 = CARTESIAN_POINT ( 'NONE',  ( -1.400000000000001910, 0.000000000000000000, 0.000000000000000000 ) ) ;
#371 = SURFACE_SIDE_STYLE ('',( #5065 ) ) ;
#372 = PRODUCT_DEFINITION_SHAPE ( 'NONE', 'NONE',  #14617 ) ;
#373 = EDGE_CURVE ( 'NONE', #10071, #11808, #3015, .T. ) ;
#374 = ORIENTED_EDGE ( 'NONE', *, *, #847, .F. ) ;
#375 = CARTESIAN_POINT ( 'NONE',  ( 637.0568832135862749, 155.4426727739092655, 210.0000000000000000 ) ) ;
#376 = ORIENTED_EDGE ( 'NONE', *, *, #2427, .F. ) ;
#377 = ORIENTED_EDGE ( 'NONE', *, *, #14177, .F. ) ;
#378 = DIRECTION ( 'NONE',  ( -1.000000000000000000, 0.000000000000000000, 0.000000000000000000 ) ) ;
#379 = VECTOR ( 'NONE', #7531, 1000.000000000000000 ) ;
#380 = AXIS2_PLACEMENT_3D ( 'NONE', #4209, #11878, #1767 ) ;
#381 = DIRECTION ( 'NONE',  ( -0.9578262852211513190, 0.2873478855663454956, -1.110223024625156540E-15 ) ) ;
#382 = VECTOR ( 'NONE', #10428, 1000.000000000000000 ) ;
#383 = DIRECTION ( 'NONE',  ( -2.312964634635740689E-15, 1.000000000000000000, 0.000000000000000000 ) ) ;
#384 = FACE_OUTER_BOUND ( 'NONE', #5110, .T. ) ;
#385 = ORIENTED_EDGE ( 'NONE', *, *, #3968, .F. ) ;
#386 = CARTESIAN_POINT ( 'NONE',  ( 10.00000000000000000, 386.5596934910894902, 210.0000000000000000 ) ) ;
#387 = LINE ( 'NONE', #4789, #930 ) ;
#388 = CARTESIAN_POINT ( 'NONE',  ( 137.1540310085880776, 355.9707293956415697, -187.0000000000000000 ) ) ;
#389 = DIRECTION ( 'NONE',  ( 1.000000000000000000, 0.000000000000000000, 0.000000000000000000 ) ) ;
#390 =( LENGTH_UNIT ( ) NAMED_UNIT ( * ) SI_UNIT ( .MILLI., .METRE. ) );
#391 = B_SPLINE_CURVE_WITH_KNOTS ( 'NONE', 3,
 ( #1032, #1097, #10197, #13582, #57 ),
 .UNSPECIFIED., .F., .F.,
 ( 4, 1, 4 ),
 ( 0.000000000000000000, 0.003752776749732567897, 0.007505553499465135794 ),
 .UNSPECIFIED. ) ;
#392 = EDGE_CURVE ( 'NONE', #3159, #7275, #4422, .T. ) ;
#393 = ORIENTED_EDGE ( 'NONE', *, *, #10167, .F. ) ;
#394 = DIRECTION ( 'NONE',  ( -0.9578262852211506528, 0.2873478855663477161, -0.000000000000000000 ) ) ;
#395 = CONICAL_SURFACE ( 'NONE', #2539, 8.542937654374687995, 1.221730476396047926 ) ;
#396 = ORIENTED_EDGE ( 'NONE', *, *, #10216, .T. ) ;
#397 = EDGE_CURVE ( 'NONE', #6493, #1729, #8054, .T. ) ;
#398 = CIRCLE ( 'NONE', #12374, 4.200000000000009059 ) ;
#399 = B_SPLINE_CURVE_WITH_KNOTS ( 'NONE', 3,
 ( #14537, #4512, #7899, #13513, #48, #4586, #8857, #13732, #2270, #11367, #13574, #5604, #1258, #113, #9970, #5755 ),
 .UNSPECIFIED., .F., .F.,
 ( 4, 3, 3, 3, 3, 4 ),
 ( -2.669610558405964892E-06, 0.000000000000000000, 5.703179328867167365E-05, 0.0001157653700801133104, 0.0001686517580788989934, 0.0002219032271218154611 ),
 .UNSPECIFIED. ) ;
#400 = DIRECTION ( 'NONE',  ( -1.000000000000000000, -0.000000000000000000, -0.000000000000000000 ) ) ;
#401 = ADVANCED_FACE ( 'NONE', ( #2445 ), #4665, .T. ) ;
#402 = DIRECTION ( 'NONE',  ( 1.000000000000000000, 0.000000000000000000, 0.000000000000000000 ) ) ;
#403 = EDGE_CURVE ( 'NONE', #12048, #8669, #5831, .T. ) ;
#404 = B_SPLINE_CURVE_WITH_KNOTS ( 'NONE', 3,
 ( #2265, #183, #10248, #7370, #11863, #11785, #14168, #411, #1689, #6194, #9441, #1819, #12981, #9584, #6332, #8391 ),
 .UNSPECIFIED., .F., .F.,
 ( 4, 2, 2, 2, 2, 2, 2, 4 ),
 ( 8.777083671441753062E-17, 0.0009429092714760194203, 0.001414363907214010374, 0.001885818542952001327, 0.002357273178689992064, 0.002828727814427983017, 0.003300182450165973971, 0.003771637085903964924 ),
 .UNSPECIFIED. ) ;
#405 = CARTESIAN_POINT ( 'NONE',  ( 1.567478505476134606E-15, 4.618802153517012066, -3.433295621305382905 ) ) ;
#406 = CIRCLE ( 'NONE', #2294, 7.000000000000006217 ) ;
#407 = EDGE_CURVE ( 'NONE', #12943, #442, #6308, .T. ) ;
#408 = AXIS2_PLACEMENT_3D ( 'NONE', #8734, #14339, #4160 ) ;
#409 = ORIENTED_EDGE ( 'NONE', *, *, #121, .F. ) ;
#410 = CARTESIAN_POINT ( 'NONE',  ( 609.6905198467529772, 186.4571330906553044, 187.4188186979287423 ) ) ;
#411 = CARTESIAN_POINT ( 'NONE',  ( 610.3331342679523459, 189.2775297294220991, -186.2537089296249349 ) ) ;
#412 = CARTESIAN_POINT ( 'NONE',  ( 3.500000000000000000, 4.618802153517012954, 0.000000000000000000 ) ) ;
#413 = DIRECTION ( 'NONE',  ( -0.9578262852211513190, 0.2873478855663453846, 0.000000000000000000 ) ) ;
#414 = ORIENTED_EDGE ( 'NONE', *, *, #14037, .F. ) ;
#415 = CARTESIAN_POINT ( 'NONE',  ( -4.000000000000000000, 0.8730739991738342143, -3.223134629628428893 ) ) ;
#416 = DIRECTION ( 'NONE',  ( 1.000000000000000000, 0.000000000000000000, 0.000000000000000000 ) ) ;
#417 = ORIENTED_EDGE ( 'NONE', *, *, #9564, .F. ) ;
#418 =( GEOMETRIC_REPRESENTATION_CONTEXT ( 3 ) GLOBAL_UNCERTAINTY_ASSIGNED_CONTEXT ( ( #11082 ) ) GLOBAL_UNIT_ASSIGNED_CONTEXT ( ( #12770, #11436, #9372 ) ) REPRESENTATION_CONTEXT ( 'NONE', 'WORKASPACE' ) );
#419 = CARTESIAN_POINT ( 'NONE',  ( 137.1540310085880776, 355.9707293956415697, -187.0000000000000000 ) ) ;
#420 = VECTOR ( 'NONE', #354, 1000.000000000000114 ) ;
#421 = AXIS2_PLACEMENT_3D ( 'NONE', #6054, #10559, #10487 ) ;
#422 = ORIENTED_EDGE ( 'NONE', *, *, #7911, .F. ) ;
#423 = ORIENTED_EDGE ( 'NONE', *, *, #14433, .T. ) ;
#424 =( NAMED_UNIT ( * ) SI_UNIT ( $, .STERADIAN. ) SOLID_ANGLE_UNIT ( ) );
#425 = DIRECTION ( 'NONE',  ( -0.9578262852211525402, 0.2873478855663419429, 0.000000000000000000 ) ) ;
#426 = EDGE_CURVE ( 'NONE', #4433, #3772, #8407, .T. ) ;
#427 = EDGE_CURVE ( 'NONE', #5340, #2146, #5598, .T. ) ;
#428 = CARTESIAN_POINT ( 'NONE',  ( 6.527192678185236296, -2.941622124011173955, 5.095038975456215091 ) ) ;
#429 = CARTESIAN_POINT ( 'NONE',  ( -8.505790995054768544, 418.4210031920615620, -184.7999999999999829 ) ) ;
#430 = EDGE_CURVE ( 'NONE', #7561, #12673, #10485, .T. ) ;
#431 = CYLINDRICAL_SURFACE ( 'NONE', #1910, 2.500000000000000444 ) ;
#432 = AXIS2_PLACEMENT_3D ( 'NONE', #1047, #4454, #8952 ) ;
#433 = VECTOR ( 'NONE', #6248, 1000.000000000000114 ) ;
#434 = PRODUCT_DEFINITION_CONTEXT ( 'detailed design', #10077, 'design' ) ;
#435 = CARTESIAN_POINT ( 'NONE',  ( 42.80949999999999278, 4.898587196589412829E-16, -4.000000000000000000 ) ) ;
#436 = ORIENTED_EDGE ( 'NONE', *, *, #13154, .F. ) ;
#437 = CARTESIAN_POINT ( 'NONE',  ( 610.0000000000000000, 10.00000000000005507, -190.0000000000000000 ) ) ;
#438 = CARTESIAN_POINT ( 'NONE',  ( -3.755786496842903988E-16, -7.505553499465146494, -6.064240316920404439 ) ) ;
#439 = CARTESIAN_POINT ( 'NONE',  ( 0.000000000000000000, 0.000000000000000000, 0.000000000000000000 ) ) ;
#440 = COLOUR_RGB ( '',1.000000000000000000, 0.9490196078431372140, 0.9098039215686274384 ) ;
#441 = CARTESIAN_POINT ( 'NONE',  ( 650.0000000000000000, 175.0000000000000568, -210.0000000000000000 ) ) ;
#442 = VERTEX_POINT ( 'NONE', #4964 ) ;
#443 = VERTEX_POINT ( 'NONE', #11657 ) ;
#444 = CARTESIAN_POINT ( 'NONE',  ( 642.3047950750122936, 158.0368908673054023, 210.0000119999999981 ) ) ;
#445 = LINE ( 'NONE', #3798, #12275 ) ;
#446 = VECTOR ( 'NONE', #14480, 1000.000000000000000 ) ;
#447 = CIRCLE ( 'NONE', #8706, 6.080745460913608902 ) ;
#448 = DIRECTION ( 'NONE',  ( 0.000000000000000000, 0.000000000000000000, 1.000000000000000000 ) ) ;
#449 = FACE_OUTER_BOUND ( 'NONE', #2353, .T. ) ;
#450 = PRESENTATION_LAYER_ASSIGNMENT (  '', '', ( #3999 ) ) ;
#451 = ORIENTED_EDGE ( 'NONE', *, *, #8325, .F. ) ;
#452 = DIRECTION ( 'NONE',  ( 0.000000000000000000, 0.000000000000000000, -1.000000000000000000 ) ) ;
#453 = CARTESIAN_POINT ( 'NONE',  ( -0.5590169943749470072, 0.000000000000000000, -5.750000000000000000 ) ) ;
#454 = CARTESIAN_POINT ( 'NONE',  ( 4.555432764205793461, -5.242992371775935467, -6.208169345099792125 ) ) ;
#455 = CIRCLE ( 'NONE', #2828, 2.199999999999757705 ) ;
#456 = AXIS2_PLACEMENT_3D ( 'NONE', #10677, #11553, #9278 ) ;
#457 = CARTESIAN_POINT ( 'NONE',  ( 3.999999999999999112, 0.000000000000000000, 3.469446951953614189E-15 ) ) ;
#458 = DIRECTION ( 'NONE',  ( -0.000000000000000000, -0.000000000000000000, -1.000000000000000000 ) ) ;
#459 = LINE ( 'NONE', #6230, #3858 ) ;
#460 = PRESENTATION_STYLE_ASSIGNMENT (( #13912 ) ) ;
#461 = ORIENTED_EDGE ( 'NONE', *, *, #7179, .T. ) ;
#462 = B_SPLINE_CURVE_WITH_KNOTS ( 'NONE', 3,
 ( #3641, #5917, #4823, #1271, #11380, #5770 ),
 .UNSPECIFIED., .F., .F.,
 ( 4, 2, 4 ),
 ( 0.003841072314098351557, 0.005765657563962180328, 0.007690242813826009098 ),
 .UNSPECIFIED. ) ;
#463 = DIRECTION ( 'NONE',  ( 0.000000000000000000, 0.000000000000000000, -1.000000000000000000 ) ) ;
#464 = EDGE_LOOP ( 'NONE', ( #13550, #7298, #1081, #14367, #9669 ) ) ;
#465 = ORIENTED_EDGE ( 'NONE', *, *, #873, .F. ) ;
#466 = AXIS2_PLACEMENT_3D ( 'NONE', #4153, #9690, #6360 ) ;
#467 = DIRECTION ( 'NONE',  ( -0.9578262852211513190, 0.2873478855663453846, -8.575812866481462478E-17 ) ) ;
#468 = AXIS2_PLACEMENT_3D ( 'NONE', #12874, #11750, #5944 ) ;
#469 = CIRCLE ( 'NONE', #11086, 8.099999999999999645 ) ;
#470 = PRESENTATION_LAYER_ASSIGNMENT (  '', '', ( #6842 ) ) ;
#471 = CARTESIAN_POINT ( 'NONE',  ( 635.0000000000000000, 160.0000000000000284, -210.0000000000000000 ) ) ;
#472 = EDGE_CURVE ( 'NONE', #11723, #11023, #398, .T. ) ;
#473 = CARTESIAN_POINT ( 'NONE',  ( 459.7035746174796031, 294.6698471414878782, 210.0000000000000000 ) ) ;
#474 = CARTESIAN_POINT ( 'NONE',  ( -9.137956343300835726, 416.3137853645748692, 184.7999999999999829 ) ) ;
#475 = AXIS2_PLACEMENT_3D ( 'NONE', #9476, #9545, #13980 ) ;
#476 = ORIENTED_EDGE ( 'NONE', *, *, #1979, .F. ) ;
#477 = CARTESIAN_POINT ( 'NONE',  ( 1.411581201560190495E-15, 4.862606272033091592, -3.745885042887436622 ) ) ;
#478 = DIRECTION ( 'NONE',  ( -0.000000000000000000, 0.000000000000000000, 1.000000000000000000 ) ) ;
#479 = VECTOR ( 'NONE', #13080, 999.9999999999998863 ) ;
#480 = DIRECTION ( 'NONE',  ( -0.000000000000000000, -0.000000000000000000, -1.000000000000000000 ) ) ;
#481 = CARTESIAN_POINT ( 'NONE',  ( -5.686050877451574337, -5.768780236673276995, 0.000000000000000000 ) ) ;
#482 =( NAMED_UNIT ( * ) SI_UNIT ( $, .STERADIAN. ) SOLID_ANGLE_UNIT ( ) );
#483 = VERTEX_POINT ( 'NONE', #435 ) ;
#484 = VECTOR ( 'NONE', #9358, 1000.000000000000000 ) ;
#485 = COLOUR_RGB ( '',0.8941176470588234615, 0.8941176470588234615, 0.8941176470588234615 ) ;
#486 = CARTESIAN_POINT ( 'NONE',  ( 2.688402820137697713, 5.953403407568487182, -0.01956314070068190455 ) ) ;
#487 = CARTESIAN_POINT ( 'NONE',  ( 6.452281807715718465, 2.898928808473057117, -5.021091983800451075 ) ) ;
#488 = VERTEX_POINT ( 'NONE', #6052 ) ;
#490 = CARTESIAN_POINT ( 'NONE',  ( -1.861313246464723443E-13, -6.204377488215742287E-13, -186.9999999999986358 ) ) ;
#489 = VECTOR ( 'NONE', #7910, 1000.000000000000114 ) ;
#491 = VECTOR ( 'NONE', #11619, 1000.000000000000000 ) ;
#492 = DIRECTION ( 'NONE',  ( 0.000000000000000000, 1.000000000000000000, 0.000000000000000000 ) ) ;
#493 = EDGE_CURVE ( 'NONE', #6798, #4861, #9598, .T. ) ;
#495 = DIRECTION ( 'NONE',  ( 0.000000000000000000, 0.000000000000000000, 1.000000000000000000 ) ) ;
#494 = VECTOR ( 'NONE', #2319, 1000.000000000000000 ) ;
#496 = EDGE_LOOP ( 'NONE', ( #8869, #13118, #1381, #11688, #8994, #12958 ) ) ;
#497 = CARTESIAN_POINT ( 'NONE',  ( -8.271276729938239853E-16, -4.452621892014642313, -2.287832656137187115 ) ) ;
#498 = EDGE_CURVE ( 'NONE', #10448, #9080, #1487, .T. ) ;
#499 = CARTESIAN_POINT ( 'NONE',  ( 635.0000000000000000, 160.0000000000000284, -210.0000000000000000 ) ) ;
#500 = CARTESIAN_POINT ( 'NONE',  ( 0.000000000000000000, -4.330127018922189208, 2.500000000000010658 ) ) ;
#501 = AXIS2_PLACEMENT_3D ( 'NONE', #42, #3395, #11489 ) ;
#502 = DIRECTION ( 'NONE',  ( -1.000000000000000000, 0.000000000000000000, 0.000000000000000000 ) ) ;
#503 = VERTEX_POINT ( 'NONE', #14036 ) ;
#504 = EDGE_CURVE ( 'NONE', #30, #10347, #1051, .T. ) ;
#505 = EDGE_LOOP ( 'NONE', ( #10225, #3201, #8699, #7735 ) ) ;
#507 = EDGE_CURVE ( 'NONE', #1236, #9769, #286, .T. ) ;
#506 = CARTESIAN_POINT ( 'NONE',  ( 455.5035746174796714, 294.6698471414878782, -210.0000000000000000 ) ) ;
#508 = COLOUR_RGB ( '',1.000000000000000000, 0.9490196078431372140, 0.9098039215686274384 ) ;
#509 = ORIENTED_EDGE ( 'NONE', *, *, #9465, .F. ) ;
#510 = DIRECTION ( 'NONE',  ( -0.5000000000000006661, 0.8660254037844382635, 0.000000000000000000 ) ) ;
#511 = DIRECTION ( 'NONE',  ( -1.000000000000000000, 0.000000000000000000, 0.000000000000000000 ) ) ;
#512 = VECTOR ( 'NONE', #1432, 1000.000000000000000 ) ;
#513 = CARTESIAN_POINT ( 'NONE',  ( 4.000000000000000000, 2.512223110932545023, -3.469391141908803711 ) ) ;
#514 = LINE ( 'NONE', #1705, #2365 ) ;
#515 = PRODUCT_DEFINITION_FORMATION_WITH_SPECIFIED_SOURCE ( 'ANY', '', #13038, .NOT_KNOWN. ) ;
#516 = DIRECTION ( 'NONE',  ( 0.000000000000000000, 0.000000000000000000, -1.000000000000000000 ) ) ;
#517 = EDGE_LOOP ( 'NONE', ( #8251, #6381, #5116, #1964 ) ) ;
#518 = EDGE_CURVE ( 'NONE', #809, #9573, #9326, .T. ) ;
#519 = FACE_OUTER_BOUND ( 'NONE', #5861, .T. ) ;
#520 = DIRECTION ( 'NONE',  ( 0.000000000000000000, 0.000000000000000000, 1.000000000000000000 ) ) ;
#521 = AXIS2_PLACEMENT_3D ( 'NONE', #8840, #3304, #12297 ) ;
#523 = EDGE_CURVE ( 'NONE', #5999, #556, #4821, .T. ) ;
#522 = FACE_OUTER_BOUND ( 'NONE', #10112, .T. ) ;
#524 = ORIENTED_EDGE ( 'NONE', *, *, #2629, .F. ) ;
#525 = VERTEX_POINT ( 'NONE', #9313 ) ;
#526 = LINE ( 'NONE', #5051, #11486 ) ;
#527 = CARTESIAN_POINT ( 'NONE',  ( 710.3801946911773939, 172.2695124801716702, -149.9999999999992610 ) ) ;
#528 = DIRECTION ( 'NONE',  ( -1.000000000000000000, 0.000000000000000000, 0.000000000000000000 ) ) ;
#529 = VECTOR ( 'NONE', #13044, 1000.000000000000000 ) ;
#530 = DIRECTION ( 'NONE',  ( 1.000000000000000000, 0.000000000000000000, 0.000000000000000000 ) ) ;
#531 = EDGE_LOOP ( 'NONE', ( #7577, #12820, #549, #541 ) ) ;
#532 = LINE ( 'NONE', #10573, #7383 ) ;
#533 = DIRECTION ( 'NONE',  ( -0.2873478855663454401, -0.9578262852211514300, -3.548540470164184620E-15 ) ) ;
#534 = CYLINDRICAL_SURFACE ( 'NONE', #9490, 4.199999999999926459 ) ;
#535 = DIRECTION ( 'NONE',  ( -0.9578262852211513190, 0.2873478855663455511, 5.916456789157588541E-31 ) ) ;
#536 = CARTESIAN_POINT ( 'NONE',  ( 650.0000000000000000, 145.0000000000000568, -210.0000000000000000 ) ) ;
#537 = CARTESIAN_POINT ( 'NONE',  ( 0.000000000000000000, 0.000000000000000000, -7.974599999999998801 ) ) ;
#538 = B_SPLINE_CURVE_WITH_KNOTS ( 'NONE', 3,
 ( #12622, #10265, #10551, #11651, #1547, #4663 ),
 .UNSPECIFIED., .F., .F.,
 ( 4, 2, 4 ),
 ( -4.604908129293502741E-06, 0.0003318387708540405283, 0.0006682824498373745670 ),
 .UNSPECIFIED. ) ;
#539 = ORIENTED_EDGE ( 'NONE', *, *, #671, .F. ) ;
#540 = DIRECTION ( 'NONE',  ( 0.000000000000000000, 1.000000000000000000, 0.000000000000000000 ) ) ;
#541 = ORIENTED_EDGE ( 'NONE', *, *, #5828, .T. ) ;
#542 = VERTEX_POINT ( 'NONE', #1550 ) ;
#543 = CARTESIAN_POINT ( 'NONE',  ( 2.999999999999999112, 4.000000000000000000, 0.000000000000000000 ) ) ;
#544 = EDGE_CURVE ( 'NONE', #1949, #5340, #2948, .T. ) ;
#545 = DIRECTION ( 'NONE',  ( 0.000000000000000000, 0.000000000000000000, -1.000000000000000000 ) ) ;
#546 = DIRECTION ( 'NONE',  ( -1.000000000000000000, 0.000000000000000000, 0.000000000000000000 ) ) ;
#547 = EDGE_CURVE ( 'NONE', #6337, #5936, #10420, .T. ) ;
#548 = CARTESIAN_POINT ( 'NONE',  ( 5.416666666666667851, 4.378239541354659536, -5.848636054922034866 ) ) ;
#549 = ORIENTED_EDGE ( 'NONE', *, *, #9465, .T. ) ;
#550 = DIRECTION ( 'NONE',  ( 0.9578262852211513190, -0.2873478855663453846, 0.000000000000000000 ) ) ;
#551 =( REPRESENTATION_RELATIONSHIP ('NONE','NONE', #2822, #748 ) REPRESENTATION_RELATIONSHIP_WITH_TRANSFORMATION ( #4045 )SHAPE_REPRESENTATION_RELATIONSHIP( ) );
#552 = CARTESIAN_POINT ( 'NONE',  ( 6.500000000000000000, 0.6659426636835951152, -5.719325464431898709 ) ) ;
#553 = PLANE ( 'NONE',  #13381 ) ;
#554 = DIRECTION ( 'NONE',  ( 0.2873478855663502141, 0.9578262852211498757, -8.036520471939056366E-30 ) ) ;
#555 =( LENGTH_UNIT ( ) NAMED_UNIT ( * ) SI_UNIT ( .MILLI., .METRE. ) );
#556 = VERTEX_POINT ( 'NONE', #3859 ) ;
#557 = FILL_AREA_STYLE ('',( #2776 ) ) ;
#558 = CARTESIAN_POINT ( 'NONE',  ( 610.3687250539534261, 189.1718658564638247, 186.1427899493634470 ) ) ;
#559 = ITEM_DEFINED_TRANSFORMATION ( 'NONE', 'NONE', #12541,  #9440 ) ;
#560 = ORIENTED_EDGE ( 'NONE', *, *, #3377, .F. ) ;
#561 = EDGE_CURVE ( 'NONE', #2165, #8693, #8490, .T. ) ;
#562 = FACE_BOUND ( 'NONE', #4810, .T. ) ;
#563 = CARTESIAN_POINT ( 'NONE',  ( 0.3572655899081607078, 2.309401076758500704, -4.000000000000000000 ) ) ;
#564 = DIRECTION ( 'NONE',  ( 1.000000000000000000, 0.000000000000000000, 0.000000000000000000 ) ) ;
#565 = ORIENTED_EDGE ( 'NONE', *, *, #4113, .T. ) ;
#566 = DIRECTION ( 'NONE',  ( -0.000000000000000000, -0.000000000000000000, -1.000000000000000000 ) ) ;
#567 = PLANE ( 'NONE',  #5021 ) ;
#568 = CARTESIAN_POINT ( 'NONE',  ( 1.274258131564866448, 3.883108878240963513, -3.220599429844046568 ) ) ;
#569 = EDGE_LOOP ( 'NONE', ( #3995, #1512, #2754, #4676 ) ) ;
#570 = CARTESIAN_POINT ( 'NONE',  ( -4.197312064133472020, -0.8182229787990021874, -3.502518405183886685 ) ) ;
#571 = ORIENTED_EDGE ( 'NONE', *, *, #126, .T. ) ;
#572 = ADVANCED_FACE ( 'NONE', ( #12850 ), #2893, .F. ) ;
#573 = ORIENTED_EDGE ( 'NONE', *, *, #7330, .T. ) ;
#574 = FACE_OUTER_BOUND ( 'NONE', #2465, .T. ) ;
#575 = CARTESIAN_POINT ( 'NONE',  ( 3.250000000000003109, -5.629165124598849879, 0.000000000000000000 ) ) ;
#576 = DIRECTION ( 'NONE',  ( 0.9578262852211509859, -0.2873478855663466613, -4.622231866529364646E-30 ) ) ;
#577 = CARTESIAN_POINT ( 'NONE',  ( 590.0000000000000000, -9.999999999999941380, -190.0000000000000000 ) ) ;
#578 = B_SPLINE_CURVE_WITH_KNOTS ( 'NONE', 3,
 ( #828, #8746, #7644, #8878, #7706, #2012, #6527, #11020 ),
 .UNSPECIFIED., .F., .F.,
 ( 4, 2, 2, 4 ),
 ( 2.465131517071352357E-07, 0.001183067374689843057, 0.001774477805458910071, 0.002365888236227977302 ),
 .UNSPECIFIED. ) ;
#579 = DIRECTION ( 'NONE',  ( -0.4113766427172328433, 0.9114654452181377708, 0.000000000000000000 ) ) ;
#580 = ORIENTED_EDGE ( 'NONE', *, *, #2612, .F. ) ;
#581 = FACE_OUTER_BOUND ( 'NONE', #7020, .T. ) ;
#582 = CARTESIAN_POINT ( 'NONE',  ( 228.5935732249375292, 306.3651924111313178, -177.6000000000005059 ) ) ;
#583 = EDGE_CURVE ( 'NONE', #4552, #13350, #10638, .T. ) ;
#584 = DIRECTION ( 'NONE',  ( 1.000000000000000000, 0.000000000000000000, 0.000000000000000000 ) ) ;
#585 = ORIENTED_EDGE ( 'NONE', *, *, #14248, .T. ) ;
#586 = ORIENTED_EDGE ( 'NONE', *, *, #12930, .F. ) ;
#587 = LINE ( 'NONE', #6359, #4201 ) ;
#588 = DIRECTION ( 'NONE',  ( 9.794481010665704304E-16, 3.264827003555234768E-15, -1.000000000000000000 ) ) ;
#589 = CARTESIAN_POINT ( 'NONE',  ( 610.0000000000000000, 0.000000000000000000, 210.0000000000000000 ) ) ;
#590 = ADVANCED_FACE ( 'NONE', ( #11807 ), #6209, .F. ) ;
#591 = EDGE_CURVE ( 'NONE', #9255, #483, #329, .T. ) ;
#592 = CARTESIAN_POINT ( 'NONE',  ( 0.000000000000000000, 0.000000000000000000, 5.000000000000000888 ) ) ;
#593 = ORIENTED_EDGE ( 'NONE', *, *, #77, .F. ) ;
#594 = ADVANCED_FACE ( 'NONE', ( #8569 ), #6567, .F. ) ;
#595 = UNCERTAINTY_MEASURE_WITH_UNIT (LENGTH_MEASURE( 1.000000000000000082E-05 ), #7441, 'distance_accuracy_value', 'NONE');
#596 = CARTESIAN_POINT ( 'NONE',  ( 630.5661054975340676, 158.1613647612965110, -210.0000000000000000 ) ) ;
#597 = CARTESIAN_POINT ( 'NONE',  ( 227.7315295682386704, 303.4917135554700280, 177.6000000000001648 ) ) ;
#598 = CARTESIAN_POINT ( 'NONE',  ( 5.000000000000000888, 0.000000000000000000, 0.000000000000000000 ) ) ;
#599 = CARTESIAN_POINT ( 'NONE',  ( 2.500000000000000000, -1.178949249685214307, 2.042000000000001592 ) ) ;
#600 = PLANE ( 'NONE',  #7043 ) ;
#601 = CARTESIAN_POINT ( 'NONE',  ( 639.0000000000000000, 164.0000000000000000, -225.5000000000000000 ) ) ;
#602 = ORIENTED_EDGE ( 'NONE', *, *, #7925, .T. ) ;
#603 = CARTESIAN_POINT ( 'NONE',  ( 3.250000000000004441, 5.629165124598849879, 0.000000000000000000 ) ) ;
#604 = VERTEX_POINT ( 'NONE', #9966 ) ;
#605 = ORIENTED_EDGE ( 'NONE', *, *, #2988, .F. ) ;
#606 = CARTESIAN_POINT ( 'NONE',  ( 451.3035746174797396, 294.6698471414878782, 210.0000000000000000 ) ) ;
#607 = EDGE_CURVE ( 'NONE', #443, #1513, #6269, .T. ) ;
#608 = DIRECTION ( 'NONE',  ( 0.000000000000000000, 0.000000000000000000, -1.000000000000000000 ) ) ;
#609 = CARTESIAN_POINT ( 'NONE',  ( 0.3117969352650125092, 2.419842229202151529, -4.999999999999999112 ) ) ;
#610 = LINE ( 'NONE', #474, #9375 ) ;
#611 = VERTEX_POINT ( 'NONE', #3108 ) ;
#612 = DIRECTION ( 'NONE',  ( 0.000000000000000000, 0.000000000000000000, -1.000000000000000000 ) ) ;
#613 = CARTESIAN_POINT ( 'NONE',  ( 639.6091003998118367, 165.9975013179864334, 210.0000119999999981 ) ) ;
#614 = CARTESIAN_POINT ( 'NONE',  ( 0.000000000000000000, 0.000000000000000000, 3.469446951953614189E-15 ) ) ;
#615 = DIRECTION ( 'NONE',  ( 0.000000000000000000, 0.000000000000000000, 1.000000000000000000 ) ) ;
#616 = ORIENTED_EDGE ( 'NONE', *, *, #591, .T. ) ;
#617 = EDGE_CURVE ( 'NONE', #4863, #2268, #5468, .T. ) ;
#618 =( NAMED_UNIT ( * ) PLANE_ANGLE_UNIT ( ) SI_UNIT ( $, .RADIAN. ) );
#619 = PLANE ( 'NONE',  #5173 ) ;
#620 = ORIENTED_EDGE ( 'NONE', *, *, #10389, .T. ) ;
#621 = B_SPLINE_CURVE_WITH_KNOTS ( 'NONE', 3,
 ( #11192, #10162, #7940, #12294, #4630, #24 ),
 .UNSPECIFIED., .F., .F.,
 ( 4, 2, 4 ),
 ( 0.000000000000000000, 0.001488912493401912647, 0.002977824986803825295 ),
 .UNSPECIFIED. ) ;
#622 = EDGE_CURVE ( 'NONE', #14203, #358, #1002, .T. ) ;
#623 = AXIS2_PLACEMENT_3D ( 'NONE', #7389, #649, #7452 ) ;
#624 = DIRECTION ( 'NONE',  ( -0.000000000000000000, -0.000000000000000000, -1.000000000000000000 ) ) ;
#625 = PRODUCT_DEFINITION_SHAPE ( 'NONE', 'NONE',  #14630 ) ;
#626 = DIRECTION ( 'NONE',  ( -0.9578262852211506528, 0.2873478855663477161, -0.000000000000000000 ) ) ;
#627 = CARTESIAN_POINT ( 'NONE',  ( -112.9080459801079144, 33.87241379403258890, 190.0000000000000000 ) ) ;
#628 = ORIENTED_EDGE ( 'NONE', *, *, #1225, .F. ) ;
#629 = CARTESIAN_POINT ( 'NONE',  ( 609.6990281814310038, 187.8427340524074225, 188.9822575857425022 ) ) ;
#630 = DIRECTION ( 'NONE',  ( -0.000000000000000000, 0.000000000000000000, 1.000000000000000000 ) ) ;
#631 = AXIS2_PLACEMENT_3D ( 'NONE', #3625, #2205, #3544 ) ;
#632 = VECTOR ( 'NONE', #8279, 1000.000000000000000 ) ;
#633 = DIRECTION ( 'NONE',  ( 1.000000000000000000, 0.000000000000000000, 0.000000000000000000 ) ) ;
#634 =( NAMED_UNIT ( * ) SI_UNIT ( $, .STERADIAN. ) SOLID_ANGLE_UNIT ( ) );
#635 = CYLINDRICAL_SURFACE ( 'NONE', #168, 0.7499999999999997780 ) ;
#636 = EDGE_LOOP ( 'NONE', ( #8796, #4569, #3020, #13957 ) ) ;
#637 = CARTESIAN_POINT ( 'NONE',  ( -4.000000000000000000, -2.512220745329312610, -3.469390707569719901 ) ) ;
#638 = DIRECTION ( 'NONE',  ( 0.000000000000000000, 0.000000000000000000, -1.000000000000000000 ) ) ;
#639 = ORIENTED_EDGE ( 'NONE', *, *, #9821, .F. ) ;
#640 = ORIENTED_EDGE ( 'NONE', *, *, #6281, .F. ) ;
#641 = ORIENTED_EDGE ( 'NONE', *, *, #544, .T. ) ;
#642 = DIRECTION ( 'NONE',  ( 0.2873478855663454401, 0.9578262852211514300, 3.831370512995697396E-15 ) ) ;
#643 = CIRCLE ( 'NONE', #14334, 7.000000000000006217 ) ;
#645 = DIRECTION ( 'NONE',  ( 0.9578262852211513190, -0.2873478855663454401, -1.972152263052529951E-31 ) ) ;
#644 = VECTOR ( 'NONE', #4252, 1000.000000000000227 ) ;
#646 = CARTESIAN_POINT ( 'NONE',  ( 639.6004632909515522, 166.0062790084377013, -210.0000000000000000 ) ) ;
#647 = EDGE_CURVE ( 'NONE', #9997, #6920, #13349, .T. ) ;
#648 = FACE_OUTER_BOUND ( 'NONE', #11384, .T. ) ;
#649 = DIRECTION ( 'NONE',  ( 0.000000000000000000, 0.000000000000000000, 1.000000000000000000 ) ) ;
#650 = ORIENTED_EDGE ( 'NONE', *, *, #6792, .F. ) ;
#651=STYLED_ITEM('',(#14681),#2645);
#652 = VECTOR ( 'NONE', #13320, 1000.000000000000000 ) ;
#653 = PLANE ( 'NONE',  #2277 ) ;
#654 = DIRECTION ( 'NONE',  ( 0.000000000000000000, 0.000000000000000000, -1.000000000000000000 ) ) ;
#655 = PRODUCT_CONTEXT ( 'NONE', #3018, 'mechanical' ) ;
#656 = CARTESIAN_POINT ( 'NONE',  ( 112.9652219749295341, 376.5507399164317803, 210.0000000000000000 ) ) ;
#657 = ORIENTED_EDGE ( 'NONE', *, *, #4005, .F. ) ;
#658 = EDGE_LOOP ( 'NONE', ( #9562, #1387, #14345, #2712 ) ) ;
#659 = DIRECTION ( 'NONE',  ( 0.9351104457158685435, 0.3543563944859322579, 0.000000000000000000 ) ) ;
#660 = DIRECTION ( 'NONE',  ( 0.000000000000000000, 0.000000000000000000, -1.000000000000000000 ) ) ;
#661 = CARTESIAN_POINT ( 'NONE',  ( 609.9641659369621038, 190.7604956903689413, -190.0000000000000568 ) ) ;
#662 = VECTOR ( 'NONE', #3204, 1000.000000000000114 ) ;
#663 = AXIS2_PLACEMENT_3D ( 'NONE', #6729, #1108, #5622 ) ;
#664 = EDGE_CURVE ( 'NONE', #7485, #11091, #11934, .T. ) ;
#665 = DIRECTION ( 'NONE',  ( -0.9578262852211518741, 0.2873478855663437748, 0.000000000000000000 ) ) ;
#666 = EDGE_LOOP ( 'NONE', ( #7423, #9314, #1783, #13496 ) ) ;
#667 = DIRECTION ( 'NONE',  ( 0.000000000000000000, -0.000000000000000000, 1.000000000000000000 ) ) ;
#668 = CARTESIAN_POINT ( 'NONE',  ( 0.000000000000000000, 0.000000000000000000, 0.000000000000000000 ) ) ;
#669 = PLANE ( 'NONE',  #940 ) ;
#670 = AXIS2_PLACEMENT_3D ( 'NONE', #13572, #3196, #13733 ) ;
#671 = EDGE_CURVE ( 'NONE', #9854, #4863, #4289, .T. ) ;
#672 = CARTESIAN_POINT ( 'NONE',  ( 8.673617379884035472E-16, 4.618802153517012954, 0.000000000000000000 ) ) ;
#673 = CARTESIAN_POINT ( 'NONE',  ( 723.8855453127954434, 217.2873478855664473, 177.5999999999999659 ) ) ;
#674 = PLANE ( 'NONE',  #14348 ) ;
#675 = EDGE_LOOP ( 'NONE', ( #11557, #8430, #2756, #7355 ) ) ;
#676 = AXIS2_PLACEMENT_3D ( 'NONE', #13441, #1099, #7762 ) ;
#677 = EDGE_CURVE ( 'NONE', #8007, #9101, #13359, .T. ) ;
#678 = LINE ( 'NONE', #11970, #4723 ) ;
#679 = CIRCLE ( 'NONE', #4453, 4.199999999999926459 ) ;
#680 = ORIENTED_EDGE ( 'NONE', *, *, #186, .T. ) ;
#681 = VERTEX_POINT ( 'NONE', #2049 ) ;
#682 = CARTESIAN_POINT ( 'NONE',  ( 636.7009106935324780, 155.5114698605638637, 210.0000000000000000 ) ) ;
#683 = EDGE_CURVE ( 'NONE', #8002, #5236, #4892, .T. ) ;
#684 = FACE_OUTER_BOUND ( 'NONE', #2603, .T. ) ;
#685 = DIRECTION ( 'NONE',  ( 0.000000000000000000, 1.000000000000000000, 0.000000000000000000 ) ) ;
#686 = TOROIDAL_SURFACE ( 'NONE', #1163, 5.100000000000000533, 0.1000000000000001582 ) ;
#687 = ORIENTED_EDGE ( 'NONE', *, *, #8817, .F. ) ;
#688 = AXIS2_PLACEMENT_3D ( 'NONE', #6223, #665, #7180 ) ;
#689 = VERTEX_POINT ( 'NONE', #9677 ) ;
#690 = LINE ( 'NONE', #5287, #12287 ) ;
#691 = CARTESIAN_POINT ( 'NONE',  ( 631.2228576472183477, 166.5533979126570330, 210.0000119999999981 ) ) ;
#692 = FACE_OUTER_BOUND ( 'NONE', #2128, .T. ) ;
#693 = CARTESIAN_POINT ( 'NONE',  ( 0.000000000000000000, 0.000000000000000000, 4.000000000000000000 ) ) ;
#694 = SURFACE_STYLE_USAGE ( .BOTH. , #13045 ) ;
#695 = CIRCLE ( 'NONE', #8953, 8.099999999999999645 ) ;
#696 = VERTEX_POINT ( 'NONE', #14184 ) ;
#698 = EDGE_CURVE ( 'NONE', #10093, #9718, #13285, .T. ) ;
#697 = AXIS2_PLACEMENT_3D ( 'NONE', #6901, #1132, #14574 ) ;
#699 = ADVANCED_FACE ( 'NONE', ( #3178 ), #5256, .F. ) ;
#700 = DIRECTION ( 'NONE',  ( 0.9578262852211514300, -0.2873478855663454401, -0.000000000000000000 ) ) ;
#701 = CARTESIAN_POINT ( 'NONE',  ( 610.0832774997078332, 190.4835367118463125, 186.9433982284626552 ) ) ;
#702 = ORIENTED_EDGE ( 'NONE', *, *, #13069, .F. ) ;
#703 = CIRCLE ( 'NONE', #8021, 4.199999999999981526 ) ;
#704 = EDGE_CURVE ( 'NONE', #7308, #3640, #8632, .T. ) ;
#705 = CIRCLE ( 'NONE', #7542, 2.500000000000000444 ) ;
#706 = ORIENTED_EDGE ( 'NONE', *, *, #5865, .T. ) ;
#707 = PLANE ( 'NONE',  #10370 ) ;
#708 = VECTOR ( 'NONE', #14194, 1000.000000000000000 ) ;
#709 = CIRCLE ( 'NONE', #9449, 4.000000000000000000 ) ;
#710 = CARTESIAN_POINT ( 'NONE',  ( 0.000000000000000000, 0.000000000000000000, -4.484454397937119197 ) ) ;
#711 = EDGE_LOOP ( 'NONE', ( #2678, #10963, #7797, #8249 ) ) ;
#712 = CARTESIAN_POINT ( 'NONE',  ( 642.0000000000000000, 235.0000000000000284, -263.5000000000000000 ) ) ;
#713 = CARTESIAN_POINT ( 'NONE',  ( 142.4540310085880606, 355.9707293956415697, -210.0000000000000000 ) ) ;
#714 = AXIS2_PLACEMENT_3D ( 'NONE', #6013, #14003, #4109 ) ;
#715 = VECTOR ( 'NONE', #5972, 1000.000000000000000 ) ;
#716 = DIRECTION ( 'NONE',  ( 0.000000000000000000, 0.000000000000000000, -1.000000000000000000 ) ) ;
#717 = ORIENTED_EDGE ( 'NONE', *, *, #3635, .T. ) ;
#718 =( NAMED_UNIT ( * ) SI_UNIT ( $, .STERADIAN. ) SOLID_ANGLE_UNIT ( ) );
#719 = FILL_AREA_STYLE ('',( #7514 ) ) ;
#720 = ORIENTED_EDGE ( 'NONE', *, *, #6916, .T. ) ;
#721 = CIRCLE ( 'NONE', #12751, 0.1000000000000002554 ) ;
#722 = ORIENTED_EDGE ( 'NONE', *, *, #12878, .F. ) ;
#723 = AXIS2_PLACEMENT_3D ( 'NONE', #11252, #12424, #13480 ) ;
#724 = ORIENTED_EDGE ( 'NONE', *, *, #11799, .T. ) ;
#725 = DIRECTION ( 'NONE',  ( -1.000000000000000000, 0.000000000000000000, 0.000000000000000000 ) ) ;
#726 = VECTOR ( 'NONE', #179, 1000.000000000000000 ) ;
#727 = FACE_OUTER_BOUND ( 'NONE', #13601, .T. ) ;
#728 = CARTESIAN_POINT ( 'NONE',  ( 639.4338945024659324, 161.8386352387035743, 211.0000000000000000 ) ) ;
#729 = VECTOR ( 'NONE', #9292, 1000.000000000000000 ) ;
#730 = DIRECTION ( 'NONE',  ( 1.000000000000000000, 0.000000000000000000, 0.000000000000000000 ) ) ;
#731 = VECTOR ( 'NONE', #4764, 1000.000000000000000 ) ;
#732 = UNCERTAINTY_MEASURE_WITH_UNIT (LENGTH_MEASURE( 1.000000000000000082E-05 ), #9644, 'distance_accuracy_value', 'NONE');
#733 = DIRECTION ( 'NONE',  ( -0.9578262852211513190, 0.2873478855663453846, -1.110223024625157329E-15 ) ) ;
#734 = VERTEX_POINT ( 'NONE', #1989 ) ;
#735 = DIRECTION ( 'NONE',  ( 1.000000000000000000, 0.000000000000000000, 0.000000000000000000 ) ) ;
#736 = CARTESIAN_POINT ( 'NONE',  ( 0.000000000000000000, 1.178949249685212974, -2.042000000000001148 ) ) ;
#737 = PRODUCT_CONTEXT ( 'NONE', #1226, 'mechanical' ) ;
#738 = CARTESIAN_POINT ( 'NONE',  ( 629.0000000000000000, 166.0000000000000284, -187.5000000000000000 ) ) ;
#739 = VERTEX_POINT ( 'NONE', #10988 ) ;
#740 = VERTEX_POINT ( 'NONE', #866 ) ;
#741 = AXIS2_PLACEMENT_3D ( 'NONE', #2991, #7488, #11983 ) ;
#742 = CARTESIAN_POINT ( 'NONE',  ( -4.000000000000000000, -2.309401076758512694, -5.000000000000000000 ) ) ;
#743 = CARTESIAN_POINT ( 'NONE',  ( 139.8040310085880833, 355.9707293956415697, 190.0000000000000000 ) ) ;
#744 = ADVANCED_FACE ( 'NONE', ( #945 ), #5383, .F. ) ;
#745 = ADVANCED_FACE ( 'NONE', ( #7680 ), #12162, .T. ) ;
#746 = CARTESIAN_POINT ( 'NONE',  ( 609.8615525982525014, 189.7413297629623514, -189.8335177487570888 ) ) ;
#747 =( REPRESENTATION_RELATIONSHIP ('NONE','NONE', #2822, #6779 ) REPRESENTATION_RELATIONSHIP_WITH_TRANSFORMATION ( #3627 )SHAPE_REPRESENTATION_RELATIONSHIP( ) );
#748 = SHAPE_REPRESENTATION ( 'handle', ( #9440 ), #10411 ) ;
#749 = DIRECTION ( 'NONE',  ( 1.000000000000000000, 0.000000000000000000, 0.000000000000000000 ) ) ;
#750 = ORIENTED_EDGE ( 'NONE', *, *, #10896, .T. ) ;
#751 = AXIS2_PLACEMENT_3D ( 'NONE', #10537, #4872, #13863 ) ;
#752 = CARTESIAN_POINT ( 'NONE',  ( 1.600000000000000089, 8.572527594031473190E-16, -7.000000000000000000 ) ) ;
#753 = DIRECTION ( 'NONE',  ( 0.000000000000000000, 0.000000000000000000, 1.000000000000000000 ) ) ;
#754 = ORIENTED_EDGE ( 'NONE', *, *, #8240, .F. ) ;
#755 = CARTESIAN_POINT ( 'NONE',  ( 153.1991633467111456, 386.6211705227183870, -190.0000000000000568 ) ) ;
#756 = DIRECTION ( 'NONE',  ( 1.000000000000000000, 0.000000000000000000, 0.000000000000000000 ) ) ;
#757 = CARTESIAN_POINT ( 'NONE',  ( 640.2500000000000000, 160.0000000000000284, -190.0000000000000000 ) ) ;
#758 = ORIENTED_EDGE ( 'NONE', *, *, #8000, .T. ) ;
#759 = AXIS2_PLACEMENT_3D ( 'NONE', #3113, #14042, #9820 ) ;
#760 = DIRECTION ( 'NONE',  ( 1.000000000000000000, 0.000000000000000000, 0.000000000000000000 ) ) ;
#761 = ORIENTED_EDGE ( 'NONE', *, *, #6990, .T. ) ;
#762 = EDGE_LOOP ( 'NONE', ( #6323, #4828, #8477, #7125 ) ) ;
#763 = DIRECTION ( 'NONE',  ( 0.000000000000000000, 0.000000000000000000, -1.000000000000000000 ) ) ;
#764 = EDGE_CURVE ( 'NONE', #11071, #8976, #2432, .T. ) ;
#765 = B_SPLINE_CURVE_WITH_KNOTS ( 'NONE', 3,
 ( #2758, #11683, #13033, #2695, #5129, #10670, #8434, #11837 ),
 .UNSPECIFIED., .F., .F.,
 ( 4, 2, 2, 4 ),
 ( 0.005725059856848641743, 0.006314084072593626612, 0.006903108288338611481, 0.008081156719828581220 ),
 .UNSPECIFIED. ) ;
#766 = AXIS2_PLACEMENT_3D ( 'NONE', #3828, #7354, #8310 ) ;
#767 = CARTESIAN_POINT ( 'NONE',  ( -10.00000000000002487, 371.6790804732684705, -184.8000000000000114 ) ) ;
#769 = EDGE_CURVE ( 'NONE', #10293, #10481, #1167, .T. ) ;
#768 = ORIENTED_EDGE ( 'NONE', *, *, #9766, .F. ) ;
#770 = ORIENTED_EDGE ( 'NONE', *, *, #10512, .T. ) ;
#771 = DIRECTION ( 'NONE',  ( 1.000000000000000000, 0.000000000000000000, 0.000000000000000000 ) ) ;
#772 = CARTESIAN_POINT ( 'NONE',  ( 6.500000000000296652, 3.350125858420170299, -6.343571411523281967 ) ) ;
#773 = CARTESIAN_POINT ( 'NONE',  ( 0.1410422978106145031, -4.700232962125109104, -3.687027686973628704 ) ) ;
#774 = CARTESIAN_POINT ( 'NONE',  ( 21.00000000000000355, 0.000000000000000000, 0.000000000000000000 ) ) ;
#775 =( NAMED_UNIT ( * ) PLANE_ANGLE_UNIT ( ) SI_UNIT ( $, .RADIAN. ) );
#776 = VECTOR ( 'NONE', #6967, 1000.000000000000000 ) ;
#777 = EDGE_LOOP ( 'NONE', ( #999, #2194, #1865, #13253 ) ) ;
#778 = DIRECTION ( 'NONE',  ( -0.9237280213470676626, -0.3830490080632388272, 0.000000000000000000 ) ) ;
#779 = CYLINDRICAL_SURFACE ( 'NONE', #2321, 7.500000000000062172 ) ;
#780 = ORIENTED_EDGE ( 'NONE', *, *, #4466, .T. ) ;
#781 = FACE_OUTER_BOUND ( 'NONE', #3795, .T. ) ;
#782 = ADVANCED_FACE ( 'NONE', ( #10186 ), #9072, .T. ) ;
#783 = VERTEX_POINT ( 'NONE', #5601 ) ;
#784 = DIRECTION ( 'NONE',  ( 1.000000000000000000, 0.000000000000000000, 0.000000000000000000 ) ) ;
#785 = ADVANCED_FACE ( 'NONE', ( #11425 ), #10715, .T. ) ;
#786 = CARTESIAN_POINT ( 'NONE',  ( 451.3035746174797396, 294.6698471414878782, 190.0000000000000568 ) ) ;
#787 = ADVANCED_FACE ( 'NONE', ( #1021 ), #12234, .F. ) ;
#788 = ORIENTED_EDGE ( 'NONE', *, *, #7769, .F. ) ;
#789 = LINE ( 'NONE', #846, #1204 ) ;
#790 = DIRECTION ( 'NONE',  ( -0.000000000000000000, -0.000000000000000000, -1.000000000000000000 ) ) ;
#791 = EDGE_CURVE ( 'NONE', #6358, #5212, #2203, .T. ) ;
#792 = CARTESIAN_POINT ( 'NONE',  ( 640.0000000000000000, 160.0000000000000284, 211.0000000000000000 ) ) ;
#793 = VERTEX_POINT ( 'NONE', #5751 ) ;
#794 = CARTESIAN_POINT ( 'NONE',  ( 237.7887055630607733, 337.0156335382104089, 182.7999999999996135 ) ) ;
#795 = CARTESIAN_POINT ( 'NONE',  ( 229.2257385731836621, 308.4724102386199434, 182.7999999999996135 ) ) ;
#796 = VERTEX_POINT ( 'NONE', #7959 ) ;
#797 = ORIENTED_EDGE ( 'NONE', *, *, #3556, .T. ) ;
#798 = CARTESIAN_POINT ( 'NONE',  ( 3.783380760145018981E-16, -7.895640089090872671, -6.564402953523720718 ) ) ;
#799 = DIRECTION ( 'NONE',  ( -1.000000000000000000, 0.000000000000000000, 0.000000000000000000 ) ) ;
#800 = CARTESIAN_POINT ( 'NONE',  ( 446.3084422793565409, 264.0194060144110608, -210.0000000000000000 ) ) ;
#801 = DIRECTION ( 'NONE',  ( 0.9578262852211514300, -0.2873478855663453846, 1.407442229263725984E-15 ) ) ;
#802 = ORIENTED_EDGE ( 'NONE', *, *, #4595, .T. ) ;
#803 = CARTESIAN_POINT ( 'NONE',  ( 6.367873360227558344, -2.886751345948134873, -5.000000000000000000 ) ) ;
#804 = CARTESIAN_POINT ( 'NONE',  ( 451.6722694765949768, 316.6998517015743460, -190.0000000000000000 ) ) ;
#805 = CARTESIAN_POINT ( 'NONE',  ( 455.5035746174796145, 294.6698471414878782, -178.5000000000000568 ) ) ;
#806 = LINE ( 'NONE', #13005, #9213 ) ;
#807 = ADVANCED_FACE ( 'NONE', ( #7749 ), #14614, .F. ) ;
#808 = VERTEX_POINT ( 'NONE', #6648 ) ;
#809 = VERTEX_POINT ( 'NONE', #3324 ) ;
#810 = DIRECTION ( 'NONE',  ( 0.000000000000000000, 1.000000000000000000, -1.224646799147353207E-16 ) ) ;
#811 = PLANE ( 'NONE',  #6832 ) ;
#812 = ADVANCED_FACE ( 'NONE', ( #2126 ), #185, .T. ) ;
#813 = PLANE ( 'NONE',  #12711 ) ;
#814 = AXIS2_PLACEMENT_3D ( 'NONE', #10708, #801, #10929 ) ;
#815 = CARTESIAN_POINT ( 'NONE',  ( -2.055025722542106692, 6.319083845363845597, -5.720331885005371930 ) ) ;
#816 = ORIENTED_EDGE ( 'NONE', *, *, #11155, .T. ) ;
#817 = CARTESIAN_POINT ( 'NONE',  ( -6.500000000000000888, 1.416734669062281959, -5.722373386996368438 ) ) ;
#818 = VERTEX_POINT ( 'NONE', #9138 ) ;
#819 = ADVANCED_FACE ( 'NONE', ( #11141 ), #13509, .T. ) ;
#820 = DIRECTION ( 'NONE',  ( 0.000000000000000000, 1.000000000000000000, 0.000000000000000000 ) ) ;
#821 = CARTESIAN_POINT ( 'NONE',  ( -1.127757440534757460, -7.231345287187099125, -6.344532336093708480 ) ) ;
#822 = CARTESIAN_POINT ( 'NONE',  ( 2.500000000000000000, -1.178949249685214307, 2.042000000000001592 ) ) ;
#823 = ORIENTED_EDGE ( 'NONE', *, *, #6899, .F. ) ;
#824 = FACE_OUTER_BOUND ( 'NONE', #10572, .T. ) ;
#825 = EDGE_LOOP ( 'NONE', ( #10283, #10217, #7029, #3003, #5201 ) ) ;
#826 = ORIENTED_EDGE ( 'NONE', *, *, #3158, .T. ) ;
#827 = DIRECTION ( 'NONE',  ( 0.000000000000000000, 0.000000000000000000, 1.000000000000000000 ) ) ;
#828 = CARTESIAN_POINT ( 'NONE',  ( -4.000000000000000000, 2.309401076758498483, -0.4999999999999927280 ) ) ;
#829 = EDGE_CURVE ( 'NONE', #12655, #11808, #12315, .T. ) ;
#830 = ORIENTED_EDGE ( 'NONE', *, *, #10724, .T. ) ;
#831 = ORIENTED_EDGE ( 'NONE', *, *, #4383, .F. ) ;
#832 = CARTESIAN_POINT ( 'NONE',  ( 6.092449800118089343, -3.827241605637789590, 3.371023086193853047 ) ) ;
#833 = ADVANCED_FACE ( 'NONE', ( #1254 ), #10098, .F. ) ;
#834 = DIRECTION ( 'NONE',  ( -0.9578262852211507639, 0.2873478855663477716, 0.000000000000000000 ) ) ;
#835 = DIRECTION ( 'NONE',  ( -1.000000000000000000, 0.000000000000000000, 0.000000000000000000 ) ) ;
#836 = DIRECTION ( 'NONE',  ( 1.000000000000000000, 0.000000000000000000, 0.000000000000000000 ) ) ;
#837 = ORIENTED_EDGE ( 'NONE', *, *, #10575, .F. ) ;
#838 = DIRECTION ( 'NONE',  ( -0.000000000000000000, -0.000000000000000000, 1.000000000000000000 ) ) ;
#839 = ITEM_DEFINED_TRANSFORMATION ( 'NONE', 'NONE', #4075,  #9440 ) ;
#840 = ORIENTED_EDGE ( 'NONE', *, *, #9284, .F. ) ;
#841 = FACE_OUTER_BOUND ( 'NONE', #13446, .T. ) ;
#842 = ORIENTED_EDGE ( 'NONE', *, *, #9433, .T. ) ;
#843 = CARTESIAN_POINT ( 'NONE',  ( 4.078421086530217288, -3.990950201428958621, 0.000000000000000000 ) ) ;
#844 = DIRECTION ( 'NONE',  ( -1.000000000000000000, -0.000000000000000000, -0.000000000000000000 ) ) ;
#845 = ORIENTED_EDGE ( 'NONE', *, *, #1115, .T. ) ;
#846 = CARTESIAN_POINT ( 'NONE',  ( 610.8620436566989156, 230.3137853645742155, -187.0000000000000000 ) ) ;
#847 = EDGE_CURVE ( 'NONE', #13246, #3959, #4647, .T. ) ;
#848 = LINE ( 'NONE', #5367, #4476 ) ;
#849 = EDGE_CURVE ( 'NONE', #611, #4450, #13643, .T. ) ;
#850 = CARTESIAN_POINT ( 'NONE',  ( 627.5000000000000000, 160.0000000000000284, -210.0000119999999981 ) ) ;
#851 =( LENGTH_UNIT ( ) NAMED_UNIT ( * ) SI_UNIT ( .MILLI., .METRE. ) );
#852 = VERTEX_POINT ( 'NONE', #8038 ) ;
#853 = EDGE_CURVE ( 'NONE', #5738, #1327, #12539, .T. ) ;
#854 = LINE ( 'NONE', #14242, #1628 ) ;
#855 = ORIENTED_EDGE ( 'NONE', *, *, #12978, .T. ) ;
#856 = ADVANCED_FACE ( 'NONE', ( #9003 ), #4603, .F. ) ;
#857 = ORIENTED_EDGE ( 'NONE', *, *, #6432, .F. ) ;
#858 = DIRECTION ( 'NONE',  ( 0.2873478855663483267, 0.9578262852211505418, 0.000000000000000000 ) ) ;
#859 = EDGE_CURVE ( 'NONE', #3582, #13126, #12261, .T. ) ;
#860 = FACE_OUTER_BOUND ( 'NONE', #1615, .T. ) ;
#861 = DIRECTION ( 'NONE',  ( -0.9578262852211513190, 0.2873478855663453846, 0.000000000000000000 ) ) ;
#862 = VECTOR ( 'NONE', #10859, 1000.000000000000114 ) ;
#863 = CIRCLE ( 'NONE', #11005, 4.199999999999926459 ) ;
#864 = PRODUCT_DEFINITION_SHAPE ( 'NONE', 'NONE',  #14641 ) ;
#865 = LINE ( 'NONE', #5382, #12271 ) ;
#866 = CARTESIAN_POINT ( 'NONE',  ( 2.000000000000005329, -3.464101615137751722, 0.000000000000000000 ) ) ;
#867 = ORIENTED_EDGE ( 'NONE', *, *, #10385, .F. ) ;
#868 = DIRECTION ( 'NONE',  ( 1.921916333308140812E-15, 6.406387777693824270E-15, -1.000000000000000000 ) ) ;
#869 = FACE_OUTER_BOUND ( 'NONE', #12744, .T. ) ;
#870 = APPLICATION_PROTOCOL_DEFINITION ( 'draft international standard', 'automotive_design', 1998, #9611 ) ;
#871 = ADVANCED_FACE ( 'NONE', ( #11787 ), #7070, .F. ) ;
#872 = AXIS2_PLACEMENT_3D ( 'NONE', #1257, #4650, #7898 ) ;
#873 = EDGE_CURVE ( 'NONE', #5188, #11030, #8324, .T. ) ;
#874 = CARTESIAN_POINT ( 'NONE',  ( -31.74999999999995737, 5.204748896376250699E-16, -4.250000000000000000 ) ) ;
#875 = AXIS2_PLACEMENT_3D ( 'NONE', #6179, #8309, #10678 ) ;
#876 = ORIENTED_EDGE ( 'NONE', *, *, #4951, .F. ) ;
#877 = ORIENTED_EDGE ( 'NONE', *, *, #6737, .T. ) ;
#878 = FILL_AREA_STYLE_COLOUR ( '', #2063 ) ;
#879 = CARTESIAN_POINT ( 'NONE',  ( 0.2500000000000002220, 0.000000000000000000, 4.250000000000000000 ) ) ;
#880 = EDGE_CURVE ( 'NONE', #1859, #4991, #1474, .T. ) ;
#881 = FACE_OUTER_BOUND ( 'NONE', #6176, .T. ) ;
#882 = FACE_BOUND ( 'NONE', #5683, .T. ) ;
#884 = ORIENTED_EDGE ( 'NONE', *, *, #11917, .F. ) ;
#883 = PRESENTATION_LAYER_ASSIGNMENT (  '', '', ( #7730 ) ) ;
#885 = VECTOR ( 'NONE', #12868, 1000.000000000000000 ) ;
#886 = DIRECTION ( 'NONE',  ( 0.000000000000000000, -1.000000000000000000, 0.000000000000000000 ) ) ;
#887 = ORIENTED_EDGE ( 'NONE', *, *, #14587, .T. ) ;
#888 = DIRECTION ( 'NONE',  ( 0.000000000000000000, 0.000000000000000000, -1.000000000000000000 ) ) ;
#889 = DIRECTION ( 'NONE',  ( -1.000000000000000000, -0.000000000000000000, -0.000000000000000000 ) ) ;
#890 = DIRECTION ( 'NONE',  ( 0.000000000000000000, 0.000000000000000000, -1.000000000000000000 ) ) ;
#891 = EDGE_LOOP ( 'NONE', ( #13342, #8061 ) ) ;
#892 = CARTESIAN_POINT ( 'NONE',  ( 0.1578711657514495215, -1.548887424847058769, 3.999999999999999112 ) ) ;
#893 = ORIENTED_EDGE ( 'NONE', *, *, #8420, .F. ) ;
#894 = ORIENTED_EDGE ( 'NONE', *, *, #607, .F. ) ;
#895 = CARTESIAN_POINT ( 'NONE',  ( 7.336184427528458230, 0.000000000000000000, 0.000000000000000000 ) ) ;
#896 = AXIS2_PLACEMENT_3D ( 'NONE', #9531, #14093, #10700 ) ;
#897 = AXIS2_PLACEMENT_3D ( 'NONE', #6006, #10504, #7188 ) ;
#898 = VECTOR ( 'NONE', #9160, 1000.000000000000114 ) ;
#899 = LINE ( 'NONE', #11699, #906 ) ;
#900 = FACE_OUTER_BOUND ( 'NONE', #12459, .T. ) ;
#901 = COLOUR_RGB ( '',1.000000000000000000, 0.9490196078431372140, 0.9098039215686274384 ) ;
#902 = VERTEX_POINT ( 'NONE', #5973 ) ;
#903 = EDGE_LOOP ( 'NONE', ( #641, #14232, #14441 ) ) ;
#904 = CARTESIAN_POINT ( 'NONE',  ( 632.5000000000001137, 160.0000000000000284, -233.5000000000000000 ) ) ;
#905 = LINE ( 'NONE', #5430, #12478 ) ;
#906 = VECTOR ( 'NONE', #6251, 1000.000000000000227 ) ;
#907 = VECTOR ( 'NONE', #4293, 999.9999999999998863 ) ;
#908 = CARTESIAN_POINT ( 'NONE',  ( -1.360585162435467455, 4.061296242128285883, -3.505054077164959203 ) ) ;
#909 = CARTESIAN_POINT ( 'NONE',  ( 631.0000000000000000, 155.9999999999999432, -225.5000000000000000 ) ) ;
#910 = DIRECTION ( 'NONE',  ( 1.000000000000000000, 0.000000000000000000, -0.000000000000000000 ) ) ;
#911 =( NAMED_UNIT ( * ) SI_UNIT ( $, .STERADIAN. ) SOLID_ANGLE_UNIT ( ) );
#912 = EDGE_LOOP ( 'NONE', ( #2980, #14447 ) ) ;
#913 = CARTESIAN_POINT ( 'NONE',  ( 609.6836880993740806, 187.1145182921505921, 188.2379512264755874 ) ) ;
#914 = EDGE_LOOP ( 'NONE', ( #13278, #11223 ) ) ;
#915 = LINE ( 'NONE', #5298, #3326 ) ;
#916 = AXIS2_PLACEMENT_3D ( 'NONE', #13048, #8314, #2933 ) ;
#917 = ORIENTED_EDGE ( 'NONE', *, *, #4871, .F. ) ;
#918 = EDGE_CURVE ( 'NONE', #12905, #9301, #11493, .T. ) ;
#919 = VECTOR ( 'NONE', #3316, 1000.000000000000000 ) ;
#920 = VECTOR ( 'NONE', #11044, 1000.000000000000114 ) ;
#921 = DIRECTION ( 'NONE',  ( -1.000000000000000000, 0.000000000000000000, 0.000000000000000000 ) ) ;
#922 = DIRECTION ( 'NONE',  ( -0.2873478855663453846, -0.9578262852211513190, -0.000000000000000000 ) ) ;
#923 = ORIENTED_EDGE ( 'NONE', *, *, #7288, .F. ) ;
#924 = CARTESIAN_POINT ( 'NONE',  ( 3.355112389629172576, -2.681727112203168950, -0.2256878752776777242 ) ) ;
#925 = CARTESIAN_POINT ( 'NONE',  ( 0.000000000000000000, 4.898587196589412829E-16, -4.000000000000000000 ) ) ;
#926 = AXIS2_PLACEMENT_3D ( 'NONE', #1440, #4912, #12807 ) ;
#927 = DIRECTION ( 'NONE',  ( -0.000000000000000000, 1.287488025362403787E-15, 1.000000000000000000 ) ) ;
#928 = ORIENTED_EDGE ( 'NONE', *, *, #12930, .T. ) ;
#929 = AXIS2_PLACEMENT_3D ( 'NONE', #5591, #6707, #6495 ) ;
#930 = VECTOR ( 'NONE', #8229, 1000.000000000000000 ) ;
#931 = VERTEX_POINT ( 'NONE', #6035 ) ;
#932 = ORIENTED_EDGE ( 'NONE', *, *, #311, .T. ) ;
#934 = FACE_OUTER_BOUND ( 'NONE', #4769, .T. ) ;
#933 = AXIS2_PLACEMENT_3D ( 'NONE', #743, #5266, #12107 ) ;
#935 = EDGE_CURVE ( 'NONE', #14514, #6201, #5231, .T. ) ;
#936 = VECTOR ( 'NONE', #1493, 1000.000000000000000 ) ;
#937 = CARTESIAN_POINT ( 'NONE',  ( 153.1991633467111456, 386.6211705227183870, 210.0000000000000000 ) ) ;
#939 = VECTOR ( 'NONE', #5652, 1000.000000000000114 ) ;
#938 = CARTESIAN_POINT ( 'NONE',  ( 628.9937209914679670, 164.6004632908573342, -210.0000000000000000 ) ) ;
#940 = AXIS2_PLACEMENT_3D ( 'NONE', #8922, #13348, #12233 ) ;
#941 = CARTESIAN_POINT ( 'NONE',  ( -0.1920286436967153787, 0.000000000000000000, 0.000000000000000000 ) ) ;
#942 = EDGE_CURVE ( 'NONE', #8737, #2165, #12678, .T. ) ;
#943 = CARTESIAN_POINT ( 'NONE',  ( 610.0000000000000000, 227.4403065089105951, 187.0000000000000000 ) ) ;
#944 = AXIS2_PLACEMENT_3D ( 'NONE', #11376, #3638, #8117 ) ;
#945 = FACE_OUTER_BOUND ( 'NONE', #496, .T. ) ;
#946 = EDGE_LOOP ( 'NONE', ( #1927, #13007, #3198 ) ) ;
#947 = VECTOR ( 'NONE', #14401, 1000.000000000000227 ) ;
#948 = CARTESIAN_POINT ( 'NONE',  ( 8.500000000000000000, 2.886751345948125547, 4.999999999999999112 ) ) ;
#949 = DIRECTION ( 'NONE',  ( 0.000000000000000000, 0.000000000000000000, 1.000000000000000000 ) ) ;
#950 = APPLICATION_PROTOCOL_DEFINITION ( 'draft international standard', 'automotive_design', 1998, #7349 ) ;
#951 = VECTOR ( 'NONE', #5253, 1000.000000000000000 ) ;
#952 = FACE_OUTER_BOUND ( 'NONE', #13047, .T. ) ;
#953 =( GEOMETRIC_REPRESENTATION_CONTEXT ( 3 ) GLOBAL_UNCERTAINTY_ASSIGNED_CONTEXT ( ( #3993 ) ) GLOBAL_UNIT_ASSIGNED_CONTEXT ( ( #2035, #12214, #5452 ) ) REPRESENTATION_CONTEXT ( 'NONE', 'WORKASPACE' ) );
#954 = ORIENTED_EDGE ( 'NONE', *, *, #1532, .T. ) ;
#955 = ORIENTED_EDGE ( 'NONE', *, *, #1459, .T. ) ;
#956 = B_SPLINE_CURVE_WITH_KNOTS ( 'NONE', 3,
 ( #12612, #7154, #2877, #2657, #2946, #11868 ),
 .UNSPECIFIED., .F., .F.,
 ( 4, 2, 4 ),
 ( 4.336808689942017736E-19, 0.001488912493401923489, 0.002977824986803846545 ),
 .UNSPECIFIED. ) ;
#957 = PRESENTATION_STYLE_ASSIGNMENT (( #12171 ) ) ;
#958 = DIRECTION ( 'NONE',  ( 0.000000000000000000, 1.000000000000000000, 3.264827003555234768E-15 ) ) ;
#959 = CARTESIAN_POINT ( 'NONE',  ( 590.0000000000000000, 10.00000000000005507, 210.0000000000000000 ) ) ;
#960 = AXIS2_PLACEMENT_3D ( 'NONE', #6772, #7955, #7892 ) ;
#961 = CIRCLE ( 'NONE', #6624, 2.700000000000000178 ) ;
#962 = PRODUCT_DEFINITION_SHAPE ( 'NONE', 'NONE',  #8642 ) ;
#963 = CARTESIAN_POINT ( 'NONE',  ( 0.000000000000000000, 0.000000000000000000, 0.000000000000000000 ) ) ;
#964 = CIRCLE ( 'NONE', #8523, 0.7499999999999997780 ) ;
#965 = ORIENTED_EDGE ( 'NONE', *, *, #10253, .F. ) ;
#966 = EDGE_CURVE ( 'NONE', #9351, #2398, #12904, .T. ) ;
#967 = DIRECTION ( 'NONE',  ( -0.2873478855663452736, -0.9578262852211514300, 0.000000000000000000 ) ) ;
#968 = B_SPLINE_CURVE_WITH_KNOTS ( 'NONE', 3,
 ( #12277, #12352, #6819, #1286, #11322 ),
 .UNSPECIFIED., .F., .F.,
 ( 4, 1, 4 ),
 ( 5.640274452250024914E-20, 0.002309401076758505356, 0.004618802153517010713 ),
 .UNSPECIFIED. ) ;
#969 = ORIENTED_EDGE ( 'NONE', *, *, #5757, .F. ) ;
#970 = EDGE_CURVE ( 'NONE', #9080, #2989, #1606, .T. ) ;
#971 = PLANE ( 'NONE',  #3973 ) ;
#972 = PRODUCT_DEFINITION ( 'UNKNOWN', '', #3122, #9597 ) ;
#973 = CARTESIAN_POINT ( 'NONE',  ( 21.00000000000000355, 2.789133085058097101E-16, -2.055000000000000160 ) ) ;
#974 = LINE ( 'NONE', #12475, #9641 ) ;
#975 = FILL_AREA_STYLE_COLOUR ( '', #508 ) ;
#976 = CIRCLE ( 'NONE', #8526, 2.649999999999985700 ) ;
#977 = CYLINDRICAL_SURFACE ( 'NONE', #1409, 6.080745460913608902 ) ;
#978 = ORIENTED_EDGE ( 'NONE', *, *, #4982, .T. ) ;
#979 = ORIENTED_EDGE ( 'NONE', *, *, #13235, .T. ) ;
#980 = DIRECTION ( 'NONE',  ( 0.000000000000000000, -1.000000000000000000, 0.000000000000000000 ) ) ;
#981 = CARTESIAN_POINT ( 'NONE',  ( 610.0000000000002274, 191.1080398579018720, 187.0000000000000284 ) ) ;
#982 = DIRECTION ( 'NONE',  ( -0.000000000000000000, -0.000000000000000000, -1.000000000000000000 ) ) ;
#983 = VECTOR ( 'NONE', #4579, 1000.000000000000227 ) ;
#984 = ORIENTED_EDGE ( 'NONE', *, *, #2925, .F. ) ;
#985 = ORIENTED_EDGE ( 'NONE', *, *, #1375, .T. ) ;
#986 = CARTESIAN_POINT ( 'NONE',  ( 609.9277849535120595, 190.4148309465319358, -190.0300000000000296 ) ) ;
#987 = CARTESIAN_POINT ( 'NONE',  ( 0.3198814748697593746, 4.434118497892183264, -0.3507732604232499107 ) ) ;
#988 = AXIS2_PLACEMENT_3D ( 'NONE', #13184, #5359, #12203 ) ;
#989 = DIRECTION ( 'NONE',  ( 0.9578262852211513190, -0.2873478855663453846, -0.000000000000000000 ) ) ;
#990 = FACE_OUTER_BOUND ( 'NONE', #11899, .T. ) ;
#991 = PLANE ( 'NONE',  #8794 ) ;
#992 = VERTEX_POINT ( 'NONE', #13950 ) ;
#993 = CARTESIAN_POINT ( 'NONE',  ( 609.6939753585367043, 187.4861613156657540, 188.5968284039610978 ) ) ;
#994 = ORIENTED_EDGE ( 'NONE', *, *, #11063, .T. ) ;
#995 = AXIS2_PLACEMENT_3D ( 'NONE', #2091, #13260, #4330 ) ;
#996 = CARTESIAN_POINT ( 'NONE',  ( 10.00000000000000000, -10.00000000000000000, 190.0000000000000000 ) ) ;
#997 = CIRCLE ( 'NONE', #9256, 5.000000000000000000 ) ;
#998 = ADVANCED_FACE ( 'NONE', ( #12835, #2716 ), #2570, .T. ) ;
#999 = ORIENTED_EDGE ( 'NONE', *, *, #2229, .F. ) ;
#1000 = EDGE_CURVE ( 'NONE', #10070, #5539, #3911, .T. ) ;
#1001 = CARTESIAN_POINT ( 'NONE',  ( -2.500000000000000444, 3.061616997868383634E-16, -25.03750572909317285 ) ) ;
#1002 = B_SPLINE_CURVE_WITH_KNOTS ( 'NONE', 3,
 ( #6499, #8853, #13073, #14469, #9816, #1834 ),
 .UNSPECIFIED., .F., .F.,
 ( 4, 2, 4 ),
 ( 0.000000000000000000, 0.001990940508721414457, 0.003981881017442828914 ),
 .UNSPECIFIED. ) ;
#1003 = CYLINDRICAL_SURFACE ( 'NONE', #11112, 7.500000000000062172 ) ;
#1004=STYLED_ITEM('',(#14681),#12340);
#1005 = VERTEX_POINT ( 'NONE', #7868 ) ;
#1006 = CARTESIAN_POINT ( 'NONE',  ( 610.1840840298345938, 189.9120001624725376, 186.6958543268122526 ) ) ;
#1007 = DIRECTION ( 'NONE',  ( -1.000000000000000000, -0.000000000000000000, -0.000000000000000000 ) ) ;
#1008 = AXIS2_PLACEMENT_3D ( 'NONE', #14417, #7766, #13089 ) ;
#1009 = DIRECTION ( 'NONE',  ( 1.000000000000000000, 0.000000000000000000, -0.000000000000000000 ) ) ;
#1010 = ORIENTED_EDGE ( 'NONE', *, *, #4852, .T. ) ;
#1011 = EDGE_CURVE ( 'NONE', #2694, #5805, #12133, .T. ) ;
#1012 = VERTEX_POINT ( 'NONE', #4251 ) ;
#1013 = ORIENTED_EDGE ( 'NONE', *, *, #8894, .F. ) ;
#1014 = DIRECTION ( 'NONE',  ( 0.9578262852211507639, -0.2873478855663477716, 0.000000000000000000 ) ) ;
#1015 = AXIS2_PLACEMENT_3D ( 'NONE', #12492, #9399, #452 ) ;
#1016 = FACE_OUTER_BOUND ( 'NONE', #7060, .T. ) ;
#1017 = CARTESIAN_POINT ( 'NONE',  ( 627.5000000000000000, 160.9948216655610622, -210.0000000000000284 ) ) ;
#1018 = LINE ( 'NONE', #10987, #13459 ) ;
#1019 = DIRECTION ( 'NONE',  ( 0.000000000000000000, 0.000000000000000000, 1.000000000000000000 ) ) ;
#1020 = DIRECTION ( 'NONE',  ( -0.000000000000000000, -0.000000000000000000, -1.000000000000000000 ) ) ;
#1021 = FACE_OUTER_BOUND ( 'NONE', #9658, .T. ) ;
#1022 = APPLICATION_CONTEXT ( 'automotive_design' ) ;
#1023 = ADVANCED_FACE ( 'NONE', ( #11243 ), #10558, .T. ) ;
#1024 = ORIENTED_EDGE ( 'NONE', *, *, #11359, .F. ) ;
#1025 = LINE ( 'NONE', #1991, #8652 ) ;
#1026 = B_SPLINE_CURVE_WITH_KNOTS ( 'NONE', 3,
 ( #1997, #8723, #14195, #3932, #1850 ),
 .UNSPECIFIED., .F., .F.,
 ( 4, 1, 4 ),
 ( 0.000000000000000000, 0.003752776749732569198, 0.007505553499465138396 ),
 .UNSPECIFIED. ) ;
#1027 = FACE_OUTER_BOUND ( 'NONE', #1102, .T. ) ;
#1028 = SHAPE_DEFINITION_REPRESENTATION ( #6637, #12910 ) ;
#1029 = CARTESIAN_POINT ( 'NONE',  ( 2.500000000000000000, 2.357898499370431722, -2.818925648462311528E-15 ) ) ;
#1030 = VERTEX_POINT ( 'NONE', #3210 ) ;
#1031 = ORIENTED_EDGE ( 'NONE', *, *, #1242, .F. ) ;
#1032 = CARTESIAN_POINT ( 'NONE',  ( -5.357619327558936585E-16, 7.505553499465137612, -6.064240316920400886 ) ) ;
#1033 = CARTESIAN_POINT ( 'NONE',  ( 610.0000000000000000, 227.4403065089105951, -187.0000000000000000 ) ) ;
#1034 = DIRECTION ( 'NONE',  ( 0.000000000000000000, 1.000000000000000000, -0.000000000000000000 ) ) ;
#1035 = ORIENTED_EDGE ( 'NONE', *, *, #8104, .F. ) ;
#1036 = EDGE_CURVE ( 'NONE', #5493, #9344, #11865, .T. ) ;
#1037 = EDGE_LOOP ( 'NONE', ( #8781, #13398, #8659, #1616 ) ) ;
#1038 = CARTESIAN_POINT ( 'NONE',  ( 443.6584422793565636, 264.0194060144110608, -190.0000000000000000 ) ) ;
#1039 = DIRECTION ( 'NONE',  ( 0.000000000000000000, -1.000000000000000000, 0.000000000000000000 ) ) ;
#1040 = ADVANCED_FACE ( 'NONE', ( #8756 ), #635, .T. ) ;
#1041 = CARTESIAN_POINT ( 'NONE',  ( 6.367873360227556567, 2.886751345948125547, 4.999999999999999112 ) ) ;
#1042 = ORIENTED_EDGE ( 'NONE', *, *, #13602, .T. ) ;
#1043 = ORIENTED_EDGE ( 'NONE', *, *, #7655, .F. ) ;
#1044 = ADVANCED_FACE ( 'NONE', ( #2017 ), #14502, .F. ) ;
#1045 = CARTESIAN_POINT ( 'NONE',  ( 635.0000000000000000, 160.0000000000000284, 215.5000000000000000 ) ) ;
#1046 = EDGE_CURVE ( 'NONE', #3037, #4895, #2875, .T. ) ;
#1047 = CARTESIAN_POINT ( 'NONE',  ( 455.5035746174796714, 294.6698471414878782, -190.0000000000000000 ) ) ;
#1048 = EDGE_CURVE ( 'NONE', #344, #12114, #2171, .T. ) ;
#1049 = CARTESIAN_POINT ( 'NONE',  ( 0.000000000000000000, 0.000000000000000000, -0.4201245229258211977 ) ) ;
#1050 = ORIENTED_EDGE ( 'NONE', *, *, #3760, .T. ) ;
#1051 = CIRCLE ( 'NONE', #11204, 4.799999999999968736 ) ;
#1052 = ORIENTED_EDGE ( 'NONE', *, *, #7592, .F. ) ;
#1053 = CARTESIAN_POINT ( 'NONE',  ( 609.7412162373094588, 188.4357741873886880, -189.3699028110927429 ) ) ;
#1054 = DIRECTION ( 'NONE',  ( -0.000000000000000000, -0.000000000000000000, 1.000000000000000000 ) ) ;
#1055 = DIRECTION ( 'NONE',  ( -0.9578262852211517631, 0.2873478855663438858, 0.000000000000000000 ) ) ;
#1056 = CARTESIAN_POINT ( 'NONE',  ( -1.655952806101422814, 3.662737355149034979, -7.623296525288699970E-18 ) ) ;
#1057 = DIRECTION ( 'NONE',  ( -0.2873478855663437193, -0.9578262852211517631, -0.000000000000000000 ) ) ;
#1058 = PRESENTATION_STYLE_ASSIGNMENT (( #12279 ) ) ;
#1059 = VERTEX_POINT ( 'NONE', #13258 ) ;
#1060 = DIRECTION ( 'NONE',  ( 0.000000000000000000, -0.5000000000000012212, -0.8660254037844380415 ) ) ;
#1061 = ADVANCED_BREP_SHAPE_REPRESENTATION ( '', ( #7422, #9440 ), #13701 ) ;
#1062 = ORIENTED_EDGE ( 'NONE', *, *, #347, .F. ) ;
#1063 = EDGE_LOOP ( 'NONE', ( #6144, #5179, #8194, #1305 ) ) ;
#1064 = CARTESIAN_POINT ( 'NONE',  ( 451.6722694765949768, 316.6998517015743460, -210.0000000000000000 ) ) ;
#1065 = EDGE_CURVE ( 'NONE', #11091, #2224, #12196, .T. ) ;
#1066 = ADVANCED_FACE ( 'NONE', ( #9586 ), #6607, .T. ) ;
#1067 = ORIENTED_EDGE ( 'NONE', *, *, #2953, .F. ) ;
#1068 = VECTOR ( 'NONE', #5913, 1000.000000000000114 ) ;
#1069 = LINE ( 'NONE', #1001, #212 ) ;
#1070 = CARTESIAN_POINT ( 'NONE',  ( 0.000000000000000000, 0.000000000000000000, -4.694516984716113228 ) ) ;
#1071 = VERTEX_POINT ( 'NONE', #4391 ) ;
#1072 = CARTESIAN_POINT ( 'NONE',  ( 455.5035746174796714, 294.6698471414878782, 187.0000000000000568 ) ) ;
#1073 = CARTESIAN_POINT ( 'NONE',  ( -10.00000000000000000, 0.000000000000000000, -190.0000000000000000 ) ) ;
#1074 = EDGE_CURVE ( 'NONE', #10137, #7536, #3365, .T. ) ;
#1075 = DIRECTION ( 'NONE',  ( 0.000000000000000000, 0.000000000000000000, -1.000000000000000000 ) ) ;
#1076 =( LENGTH_UNIT ( ) NAMED_UNIT ( * ) SI_UNIT ( .MILLI., .METRE. ) );
#1077 =( LENGTH_UNIT ( ) NAMED_UNIT ( * ) SI_UNIT ( .MILLI., .METRE. ) );
#1078 = VERTEX_POINT ( 'NONE', #7372 ) ;
#1079 = EDGE_CURVE ( 'NONE', #7687, #12048, #11107, .T. ) ;
#1080 = DIRECTION ( 'NONE',  ( 0.8191520442889875797, 0.000000000000000000, 0.5735764363510522656 ) ) ;
#1081 = ORIENTED_EDGE ( 'NONE', *, *, #4008, .T. ) ;
#1082 = EDGE_LOOP ( 'NONE', ( #12851, #11532 ) ) ;
#1083 = CARTESIAN_POINT ( 'NONE',  ( 1.399999999999998579, 0.000000000000000000, 0.000000000000000000 ) ) ;
#1084 = FACE_OUTER_BOUND ( 'NONE', #6931, .T. ) ;
#1085 = CARTESIAN_POINT ( 'NONE',  ( 630.3996772907336208, 166.0061384269410212, -210.0000000000000284 ) ) ;
#1086 = CARTESIAN_POINT ( 'NONE',  ( 635.0000000000000000, 235.0000000000000284, -233.5000000000000000 ) ) ;
#1087 = DIRECTION ( 'NONE',  ( -0.000000000000000000, 0.000000000000000000, 1.000000000000000000 ) ) ;
#1088 = CARTESIAN_POINT ( 'NONE',  ( 21.00000000000000355, 2.516649172247811061E-16, -2.055000000000000160 ) ) ;
#1089 = DIRECTION ( 'NONE',  ( -0.000000000000000000, -0.000000000000000000, 1.000000000000000000 ) ) ;
#1090 = ORIENTED_EDGE ( 'NONE', *, *, #6198, .F. ) ;
#1091 = DIRECTION ( 'NONE',  ( 1.000000000000000000, 0.000000000000000000, -0.000000000000000000 ) ) ;
#1092 = DIRECTION ( 'NONE',  ( -1.000000000000000000, 0.000000000000000000, 0.000000000000000000 ) ) ;
#1093 = SHAPE_DEFINITION_REPRESENTATION ( #10785, #5933 ) ;
#1094 = DIRECTION ( 'NONE',  ( 0.000000000000000000, 0.000000000000000000, 1.000000000000000000 ) ) ;
#1095 = EDGE_LOOP ( 'NONE', ( #8108, #3138 ) ) ;
#1096 = EDGE_LOOP ( 'NONE', ( #2757, #837, #2555, #2386, #1528, #4159 ) ) ;
#1097 = CARTESIAN_POINT ( 'NONE',  ( -1.083333333333333259, 6.880090707843040221, -5.848636054922037530 ) ) ;
#1099 = DIRECTION ( 'NONE',  ( -0.000000000000000000, -0.000000000000000000, 1.000000000000000000 ) ) ;
#1098 = AXIS2_PLACEMENT_3D ( 'NONE', #169, #2550, #9503 ) ;
#1100 = ADVANCED_FACE ( 'NONE', ( #1755 ), #2999, .F. ) ;
#1101 = CARTESIAN_POINT ( 'NONE',  ( -5.727634848077285845, 4.575561887448583498, -6.326622577870772979 ) ) ;
#1102 = EDGE_LOOP ( 'NONE', ( #5350, #8471, #4315, #12302 ) ) ;
#1103 = DIRECTION ( 'NONE',  ( 1.000000000000000000, 0.000000000000000000, -0.000000000000000000 ) ) ;
#1104 = ORIENTED_EDGE ( 'NONE', *, *, #7956, .T. ) ;
#1105=STYLED_ITEM('',(#14681),#2215);
#1106 = VECTOR ( 'NONE', #4618, 1000.000000000000000 ) ;
#1107 = CARTESIAN_POINT ( 'NONE',  ( 1.567478505476134606E-15, 4.618802153517012066, -3.433295621305382905 ) ) ;
#1108 = DIRECTION ( 'NONE',  ( 1.000000000000000000, 0.000000000000000000, 0.000000000000000000 ) ) ;
#1109 =( NAMED_UNIT ( * ) PLANE_ANGLE_UNIT ( ) SI_UNIT ( $, .RADIAN. ) );
#1110 = DIRECTION ( 'NONE',  ( 0.000000000000000000, 0.000000000000000000, -1.000000000000000000 ) ) ;
#1111 = ORIENTED_EDGE ( 'NONE', *, *, #1647, .T. ) ;
#1112 = ORIENTED_EDGE ( 'NONE', *, *, #14048, .T. ) ;
#1113 = CARTESIAN_POINT ( 'NONE',  ( 4.197393957002303999, -0.4069871074557456780, -3.503767560748925813 ) ) ;
#1114 = DIRECTION ( 'NONE',  ( -0.4113766427172328433, 0.9114654452181377708, 0.000000000000000000 ) ) ;
#1115 = EDGE_CURVE ( 'NONE', #10699, #12031, #8189, .T. ) ;
#1116 = MECHANICAL_DESIGN_GEOMETRIC_PRESENTATION_REPRESENTATION (  '', ( #7730 ), #6784 ) ;
#1117 = DIRECTION ( 'NONE',  ( -1.000000000000000000, -0.000000000000000000, -0.000000000000000000 ) ) ;
#1118 = VECTOR ( 'NONE', #1505, 1000.000000000000114 ) ;
#1119 = EDGE_CURVE ( 'NONE', #14292, #9101, #13687, .T. ) ;
#1120 = VERTEX_POINT ( 'NONE', #9039 ) ;
#1121 = ORIENTED_EDGE ( 'NONE', *, *, #2407, .T. ) ;
#1122 = CARTESIAN_POINT ( 'NONE',  ( 609.8579287883226243, 189.7296425882048823, -189.8646579186752774 ) ) ;
#1123 = CARTESIAN_POINT ( 'NONE',  ( 10.00000000000000000, 386.5596934910894902, 210.0000000000000000 ) ) ;
#1124 = EDGE_CURVE ( 'NONE', #10210, #9473, #7995, .T. ) ;
#1125 = DIRECTION ( 'NONE',  ( 0.000000000000000000, 0.000000000000000000, 1.000000000000000000 ) ) ;
#1126 = LINE ( 'NONE', #5639, #9616 ) ;
#1127 = LINE ( 'NONE', #1287, #9270 ) ;
#1128 = FILL_AREA_STYLE_COLOUR ( '', #9466 ) ;
#1129 = ORIENTED_EDGE ( 'NONE', *, *, #11458, .T. ) ;
#1130 = AXIS2_PLACEMENT_3D ( 'NONE', #14176, #6265, #9591 ) ;
#1131 = ADVANCED_FACE ( 'NONE', ( #11459 ), #3428, .F. ) ;
#1132 = DIRECTION ( 'NONE',  ( 1.000000000000000000, 0.000000000000000000, 0.000000000000000000 ) ) ;
#1133 = VECTOR ( 'NONE', #3132, 1000.000000000000000 ) ;
#1134 = CIRCLE ( 'NONE', #11736, 2.041999999999999815 ) ;
#1135 = VERTEX_POINT ( 'NONE', #1352 ) ;
#1136 = ORIENTED_EDGE ( 'NONE', *, *, #3332, .T. ) ;
#1137 = CARTESIAN_POINT ( 'NONE',  ( 6.323268674612417151, -2.010012106700867385, -5.000000000000872191 ) ) ;
#1138 = VERTEX_POINT ( 'NONE', #12577 ) ;
#1139 = CARTESIAN_POINT ( 'NONE',  ( -31.74999999999995737, 0.000000000000000000, 0.000000000000000000 ) ) ;
#1140 = DIRECTION ( 'NONE',  ( 0.9578262852211485434, -0.2873478855663546550, 0.000000000000000000 ) ) ;
#1141 = AXIS2_PLACEMENT_3D ( 'NONE', #1241, #5744, #10241 ) ;
#1142 = AXIS2_PLACEMENT_3D ( 'NONE', #1745, #6320, #10822 ) ;
#1143 = ORIENTED_EDGE ( 'NONE', *, *, #9016, .T. ) ;
#1144 = DIRECTION ( 'NONE',  ( 1.000000000000000000, 0.000000000000000000, 0.000000000000000000 ) ) ;
#1145 = CARTESIAN_POINT ( 'NONE',  ( 635.0000000000000000, 160.0000000000000284, 190.0000000000000284 ) ) ;
#1146 = EDGE_CURVE ( 'NONE', #503, #13396, #5852, .T. ) ;
#1147 = CARTESIAN_POINT ( 'NONE',  ( 0.000000000000000000, 0.000000000000000000, -1.000000000000000000 ) ) ;
#1148 = FACE_OUTER_BOUND ( 'NONE', #13299, .T. ) ;
#1149 = ORIENTED_EDGE ( 'NONE', *, *, #11070, .T. ) ;
#1150 = AXIS2_PLACEMENT_3D ( 'NONE', #673, #6229, #6519 ) ;
#1151 = ADVANCED_FACE ( 'NONE', ( #13542 ), #5638, .F. ) ;
#1152 = CARTESIAN_POINT ( 'NONE',  ( 459.3348797583643091, 272.6398425814014104, -190.0000000000000000 ) ) ;
#1153 = B_SPLINE_CURVE_WITH_KNOTS ( 'NONE', 3,
 ( #6799, #13590, #8056, #7914, #10271 ),
 .UNSPECIFIED., .F., .F.,
 ( 4, 1, 4 ),
 ( 0.000000000000000000, 0.002309401076758505790, 0.004618802153517011580 ),
 .UNSPECIFIED. ) ;
#1154 = ORIENTED_EDGE ( 'NONE', *, *, #7723, .F. ) ;
#1155 = CIRCLE ( 'NONE', #6814, 0.1000000000000002554 ) ;
#1156 = CIRCLE ( 'NONE', #13898, 4.199999999999981526 ) ;
#1157 = ORIENTED_EDGE ( 'NONE', *, *, #5120, .F. ) ;
#1158 = DIRECTION ( 'NONE',  ( -0.000000000000000000, -0.000000000000000000, -1.000000000000000000 ) ) ;
#1159 = CARTESIAN_POINT ( 'NONE',  ( -20.63749999999999929, 0.000000000000000000, 0.000000000000000000 ) ) ;
#1160 = MECHANICAL_DESIGN_GEOMETRIC_PRESENTATION_REPRESENTATION (  '', ( #3274 ), #2339 ) ;
#1161 = CARTESIAN_POINT ( 'NONE',  ( 3.999999999999999112, -0.3979232138631231819, -5.929230630780099908E-17 ) ) ;
#1162 = FACE_OUTER_BOUND ( 'NONE', #3028, .T. ) ;
#1163 = AXIS2_PLACEMENT_3D ( 'NONE', #6324, #6111, #1595 ) ;
#1164 = AXIS2_PLACEMENT_3D ( 'NONE', #12417, #11320, #11395 ) ;
#1165 = DIRECTION ( 'NONE',  ( 1.000000000000000000, 0.000000000000000000, 0.000000000000000000 ) ) ;
#1166 = CARTESIAN_POINT ( 'NONE',  ( 7.336184427528458230, 9.926022037524705097E-16, 8.105212085995399107 ) ) ;
#1167 = LINE ( 'NONE', #4581, #5578 ) ;
#1168 = ORIENTED_EDGE ( 'NONE', *, *, #11531, .F. ) ;
#1169 = CARTESIAN_POINT ( 'NONE',  ( 3.500000000000000000, 0.000000000000000000, 0.000000000000000000 ) ) ;
#1170 = CARTESIAN_POINT ( 'NONE',  ( 446.3084422793565409, 264.0194060144110608, -190.0000000000000000 ) ) ;
#1171 = PRODUCT_CONTEXT ( 'NONE', #13377, 'mechanical' ) ;
#1172 = ORIENTED_EDGE ( 'NONE', *, *, #4383, .T. ) ;
#1173 = CONICAL_SURFACE ( 'NONE', #6364, 8.105212085995399107, 1.221730476396037490 ) ;
#1174 = VECTOR ( 'NONE', #12504, 1000.000000000000114 ) ;
#1175 = DIRECTION ( 'NONE',  ( 1.000000000000000000, 0.000000000000000000, 0.000000000000000000 ) ) ;
#1176 = EDGE_LOOP ( 'NONE', ( #12389, #12490, #761, #12684 ) ) ;
#1177 = ORIENTED_EDGE ( 'NONE', *, *, #3606, .F. ) ;
#1178 = CARTESIAN_POINT ( 'NONE',  ( 611.4942090049449916, 232.4210031920605388, 187.0000000000000000 ) ) ;
#1179 = AXIS2_PLACEMENT_3D ( 'NONE', #9634, #2921, #1797 ) ;
#1180 = CIRCLE ( 'NONE', #3319, 2.700000000000000622 ) ;
#1181 = LINE ( 'NONE', #959, #202 ) ;
#1182 = CIRCLE ( 'NONE', #4025, 2.649999999999985700 ) ;
#1183 = CARTESIAN_POINT ( 'NONE',  ( 650.0000000000000000, 145.0000000000000568, -190.0000000000000000 ) ) ;
#1184 = AXIS2_PLACEMENT_3D ( 'NONE', #4149, #6216, #4000 ) ;
#1185 = CARTESIAN_POINT ( 'NONE',  ( 451.6722694765949768, 316.6998517015743460, 190.0000000000000000 ) ) ;
#1186 = ORIENTED_EDGE ( 'NONE', *, *, #302, .F. ) ;
#1187 = VECTOR ( 'NONE', #4576, 1000.000000000000000 ) ;
#1188 = CARTESIAN_POINT ( 'NONE',  ( 6.534838248920896930, 2.951765777552409986, -5.112608298763837489 ) ) ;
#1189 = DIRECTION ( 'NONE',  ( 0.000000000000000000, 1.000000000000000000, 0.000000000000000000 ) ) ;
#1190 =( NAMED_UNIT ( * ) SI_UNIT ( $, .STERADIAN. ) SOLID_ANGLE_UNIT ( ) );
#1191 = ADVANCED_FACE ( 'NONE', ( #7929 ), #11961, .F. ) ;
#1192 = CYLINDRICAL_SURFACE ( 'NONE', #2355, 3.399999999999999911 ) ;
#1193 = EDGE_CURVE ( 'NONE', #818, #8680, #12496, .T. ) ;
#1194 = EDGE_LOOP ( 'NONE', ( #13478, #6976 ) ) ;
#1195 = ORIENTED_EDGE ( 'NONE', *, *, #13922, .T. ) ;
#1196 = AXIS2_PLACEMENT_3D ( 'NONE', #8787, #1988, #730 ) ;
#1197 = DIRECTION ( 'NONE',  ( 0.000000000000000000, 0.000000000000000000, 1.000000000000000000 ) ) ;
#1198 = VECTOR ( 'NONE', #12811, 1000.000000000000114 ) ;
#1199 = CARTESIAN_POINT ( 'NONE',  ( 2.999999999999999112, 0.000000000000000000, 0.000000000000000000 ) ) ;
#1200 = CIRCLE ( 'NONE', #13231, 2.100000000000000089 ) ;
#1201 = PRESENTATION_LAYER_ASSIGNMENT (  '', '', ( #6170 ) ) ;
#1202 = CARTESIAN_POINT ( 'NONE',  ( -4.198928548860774157, 0.8158838809860065044, -3.526471437616918170 ) ) ;
#1203 = EDGE_LOOP ( 'NONE', ( #10875, #5229, #6450, #4248, #6568 ) ) ;
#1204 = VECTOR ( 'NONE', #5366, 1000.000000000000227 ) ;
#1205 = ORIENTED_EDGE ( 'NONE', *, *, #4135, .F. ) ;
#1206 = CARTESIAN_POINT ( 'NONE',  ( 610.0835668916889745, 190.4817695994259736, -186.9427398886703315 ) ) ;
#1207 = CARTESIAN_POINT ( 'NONE',  ( 1.144235203016666258, 3.958177651039090250, -0.09382832055445661235 ) ) ;
#1208 = CIRCLE ( 'NONE', #13243, 7.500000000000062172 ) ;
#1209 = CARTESIAN_POINT ( 'NONE',  ( 6.506987859255520590, 5.850751062354591525, -2.486036146584983242E-15 ) ) ;
#1210 = DIRECTION ( 'NONE',  ( -1.000000000000000000, -0.000000000000000000, -0.000000000000000000 ) ) ;
#1211 = CARTESIAN_POINT ( 'NONE',  ( 148.9991633467111569, 386.6211705227183870, 210.0000000000000000 ) ) ;
#1212 =( LENGTH_UNIT ( ) NAMED_UNIT ( * ) SI_UNIT ( .MILLI., .METRE. ) );
#1213 = B_SPLINE_SURFACE_WITH_KNOTS ( 'NONE', 1, 3, ( 
 ( #6681, #986, #9036, #1053, #5504, #11241, #5562, #10061, #7866, #14568 ),
 ( #2300, #4459, #1122, #9178, #5635, #6812, #75, #13540, #3426, #12493 ),
 ( #9102, #13685, #1206, #10218, #3497, #7991, #6893, #8289, #4835, #13761 ),
 ( #12799, #1502, #10658, #7031, #11533, #7115, #13904, #366, #13824, #1643 ) ),
 .UNSPECIFIED., .F., .F., .F.,
 ( 2, 1, 1, 2 ),
 ( 4, 2, 2, 2, 4 ),
 ( -0.01000000000000000021, 0.000000000000000000, 1.000000000000000000, 1.010099999999999998 ),
 ( 0.000000000000000000, 0.2500000000000000000, 0.5000000000000000000, 0.7500000000000000000, 1.000000000000000000 ),
 .UNSPECIFIED. ) ;
#1214 = EDGE_CURVE ( 'NONE', #7124, #3179, #229, .T. ) ;
#1215 = ORIENTED_EDGE ( 'NONE', *, *, #9273, .T. ) ;
#1216 = CARTESIAN_POINT ( 'NONE',  ( 0.000000000000000000, 0.000000000000000000, 0.000000000000000000 ) ) ;
#1217 = EDGE_LOOP ( 'NONE', ( #14260, #12001, #10390, #9108 ) ) ;
#1218 = VERTEX_POINT ( 'NONE', #11321 ) ;
#1219 = CARTESIAN_POINT ( 'NONE',  ( 6.390983168987730778, -3.014662706507984513, -5.000000000000000000 ) ) ;
#1220 = VECTOR ( 'NONE', #13865, 1000.000000000000114 ) ;
#1221 = ORIENTED_EDGE ( 'NONE', *, *, #12699, .T. ) ;
#1222 = CIRCLE ( 'NONE', #741, 0.7499999999999997780 ) ;
#1223 = EDGE_CURVE ( 'NONE', #11111, #2958, #8567, .T. ) ;
#1224 = CARTESIAN_POINT ( 'NONE',  ( 5.000000000000002665, 3.306546357697854226E-16, 2.700000000000000622 ) ) ;
#1225 = EDGE_CURVE ( 'NONE', #852, #13547, #7265, .T. ) ;
#1226 = APPLICATION_CONTEXT ( 'automotive_design' ) ;
#1227 = DIRECTION ( 'NONE',  ( -0.2873478855663453846, -0.9578262852211513190, -0.000000000000000000 ) ) ;
#1228 = AXIS2_PLACEMENT_3D ( 'NONE', #7615, #14188, #4146 ) ;
#1229 = EDGE_LOOP ( 'NONE', ( #830, #13146 ) ) ;
#1230 = CARTESIAN_POINT ( 'NONE',  ( 0.1996310553826622369, 1.947030205581111728, 4.999999999999997335 ) ) ;
#1231 = CARTESIAN_POINT ( 'NONE',  ( -1.500000000000001332, 0.000000000000000000, 0.000000000000000000 ) ) ;
#1232 = CARTESIAN_POINT ( 'NONE',  ( 1.250000000000000000, -6.429618962271402616, -1.000000000000000000 ) ) ;
#1233 = LINE ( 'NONE', #1302, #40 ) ;
#1234 = CIRCLE ( 'NONE', #4306, 3.999999999999999112 ) ;
#1235 = ADVANCED_FACE ( 'NONE', ( #5784, #148 ), #4690, .T. ) ;
#1236 = VERTEX_POINT ( 'NONE', #9402 ) ;
#1237 = DIRECTION ( 'NONE',  ( 0.9578262852211507639, -0.2873478855663477716, 0.000000000000000000 ) ) ;
#1238 = VERTEX_POINT ( 'NONE', #2976 ) ;
#1239 = DIRECTION ( 'NONE',  ( -3.340694023494469140E-16, 4.069768234201303760E-15, 1.000000000000000000 ) ) ;
#1240 = EDGE_LOOP ( 'NONE', ( #11426, #3550, #720, #5987 ) ) ;
#1241 = CARTESIAN_POINT ( 'NONE',  ( -8.505790995054995918, 418.4210031920614483, 184.7999999999999829 ) ) ;
#1242 = EDGE_CURVE ( 'NONE', #72, #3152, #10578, .T. ) ;
#1243 = EDGE_CURVE ( 'NONE', #13718, #4881, #11032, .T. ) ;
#1244 = CARTESIAN_POINT ( 'NONE',  ( 638.7885571598276329, 153.4512226587835642, -210.0000000000000000 ) ) ;
#1245 = AXIS2_PLACEMENT_3D ( 'NONE', #481, #1523, #8231 ) ;
#1246 = DIRECTION ( 'NONE',  ( 1.000000000000000000, 0.000000000000000000, 0.000000000000000000 ) ) ;
#1248 = EDGE_CURVE ( 'NONE', #4325, #1327, #12801, .T. ) ;
#1247 = AXIS2_PLACEMENT_3D ( 'NONE', #5486, #5271, #5189 ) ;
#1249 = CARTESIAN_POINT ( 'NONE',  ( 112.9652219749295341, 376.5507399164317803, 210.0000000000000000 ) ) ;
#1250 = AXIS2_PLACEMENT_3D ( 'NONE', #11877, #11805, #10705 ) ;
#1251 = DIRECTION ( 'NONE',  ( -0.9578262852211513190, 0.2873478855663453846, 0.000000000000000000 ) ) ;
#1252 = DIRECTION ( 'NONE',  ( -1.000000000000000000, 0.000000000000000000, 0.000000000000000000 ) ) ;
#1253 = B_SPLINE_CURVE_WITH_KNOTS ( 'NONE', 3,
 ( #6029, #10242, #10312, #9289, #3681, #8161 ),
 .UNSPECIFIED., .F., .F.,
 ( 4, 2, 4 ),
 ( 0.003358874760055550156, 0.004541967308452096383, 0.005725059856848641743 ),
 .UNSPECIFIED. ) ;
#1254 = FACE_OUTER_BOUND ( 'NONE', #6553, .T. ) ;
#1255 = ORIENTED_EDGE ( 'NONE', *, *, #4794, .T. ) ;
#1256 = DIRECTION ( 'NONE',  ( 1.000000000000000000, 0.000000000000000000, 0.000000000000000000 ) ) ;
#1257 = CARTESIAN_POINT ( 'NONE',  ( 611.4942090049451053, 232.4210031920599420, -184.7999999999999829 ) ) ;
#1258 = CARTESIAN_POINT ( 'NONE',  ( 6.420058897733094128, -5.782965130189197112, 5.182398524903814613E-16 ) ) ;
#1259 = ORIENTED_EDGE ( 'NONE', *, *, #5103, .T. ) ;
#1260 = VECTOR ( 'NONE', #3658, 1000.000000000000000 ) ;
#1261 = FACE_OUTER_BOUND ( 'NONE', #8689, .T. ) ;
#1262 = ORIENTED_EDGE ( 'NONE', *, *, #8034, .T. ) ;
#1263 = ORIENTED_EDGE ( 'NONE', *, *, #6739, .F. ) ;
#1264 = SURFACE_STYLE_USAGE ( .BOTH. , #8178 ) ;
#1265 = FACE_OUTER_BOUND ( 'NONE', #4449, .T. ) ;
#1266 = CARTESIAN_POINT ( 'NONE',  ( 4.999999999999997335, 0.000000000000000000, 0.000000000000000000 ) ) ;
#1267 = LINE ( 'NONE', #577, #4034 ) ;
#1268 = CARTESIAN_POINT ( 'NONE',  ( 6.242800618755250497, -4.918813924287368522, -1.690830708135581784 ) ) ;
#1269 = ORIENTED_EDGE ( 'NONE', *, *, #6620, .T. ) ;
#1270 = EDGE_CURVE ( 'NONE', #14191, #3125, #7474, .T. ) ;
#1271 = CARTESIAN_POINT ( 'NONE',  ( -1.058054217398698871, 6.894685612232779981, -0.3576316571898437990 ) ) ;
#1272 = DIRECTION ( 'NONE',  ( 1.387778780781446464E-15, -2.775557561562892929E-15, 1.000000000000000000 ) ) ;
#1273 = EDGE_CURVE ( 'NONE', #12403, #5365, #10729, .T. ) ;
#1274 = CARTESIAN_POINT ( 'NONE',  ( 627.2408731339806991, 284.9098836221797342, 187.0000000000001990 ) ) ;
#1275 = ORIENTED_EDGE ( 'NONE', *, *, #3249, .T. ) ;
#1276 = ORIENTED_EDGE ( 'NONE', *, *, #5646, .T. ) ;
#1277 = CARTESIAN_POINT ( 'NONE',  ( 630.3908996001882770, 154.0024986820136803, 210.0000119999999981 ) ) ;
#1278 = CYLINDRICAL_SURFACE ( 'NONE', #2591, 5.000000000000004441 ) ;
#1279 = CARTESIAN_POINT ( 'NONE',  ( 7.900000000000002132, 9.674709713264094059E-16, -7.900000000000002132 ) ) ;
#1280 = CARTESIAN_POINT ( 'NONE',  ( 4.000000000000000000, -0.8732470631449981147, -3.223155494240760088 ) ) ;
#1281 = EDGE_LOOP ( 'NONE', ( #4973, #2971, #14599, #4787, #9806, #8332, #7169, #8113, #6262, #12089, #4623, #4827, #11001, #11503, #12582, #10546 ) ) ;
#1282 = EDGE_LOOP ( 'NONE', ( #8949, #7647, #11738, #7924 ) ) ;
#1283 = FACE_OUTER_BOUND ( 'NONE', #8141, .T. ) ;
#1284 = CARTESIAN_POINT ( 'NONE',  ( 0.000000000000000000, 0.000000000000000000, -0.2800830152838844622 ) ) ;
#1285 = DIRECTION ( 'NONE',  ( -0.2873478855663483267, -0.9578262852211505418, -5.337610695313246651E-15 ) ) ;
#1286 = CARTESIAN_POINT ( 'NONE',  ( 3.333333333333335702, -2.694301256218268215, -3.300726591567084256 ) ) ;
#1287 = CARTESIAN_POINT ( 'NONE',  ( -20.63749999999999929, 6.123233995736766282E-16, 5.000000000000000000 ) ) ;
#1288 = SURFACE_STYLE_USAGE ( .BOTH. , #11399 ) ;
#1289 = ORIENTED_EDGE ( 'NONE', *, *, #8696, .F. ) ;
#1290 = DIRECTION ( 'NONE',  ( -0.000000000000000000, -0.000000000000000000, 1.000000000000000000 ) ) ;
#1291 = ORIENTED_EDGE ( 'NONE', *, *, #25, .F. ) ;
#1292 = ORIENTED_EDGE ( 'NONE', *, *, #7379, .F. ) ;
#1293 = DIRECTION ( 'NONE',  ( 0.000000000000000000, -0.5000000000000018874, -0.8660254037844375974 ) ) ;
#1294 = DIRECTION ( 'NONE',  ( -1.000000000000000000, -9.498873539028489960E-17, -0.000000000000000000 ) ) ;
#1295 = EDGE_CURVE ( 'NONE', #10237, #8326, #1789, .T. ) ;
#1296 = B_SPLINE_CURVE_WITH_KNOTS ( 'NONE', 3,
 ( #6642, #11136, #2043, #3236, #14607, #4499 ),
 .UNSPECIFIED., .F., .F.,
 ( 4, 2, 4 ),
 ( 0.005511122051665403969, 0.007432374760074392586, 0.009353627468483380336 ),
 .UNSPECIFIED. ) ;
#1297 = PLANE ( 'NONE',  #3818 ) ;
#1298 = ORIENTED_EDGE ( 'NONE', *, *, #3771, .T. ) ;
#1299 = PLANE ( 'NONE',  #13009 ) ;
#1300 = DIRECTION ( 'NONE',  ( 1.000000000000000000, 0.000000000000000000, 0.000000000000000000 ) ) ;
#1301 = DIRECTION ( 'NONE',  ( 0.000000000000000000, -1.000000000000000000, 0.000000000000000000 ) ) ;
#1302 = CARTESIAN_POINT ( 'NONE',  ( -9.511508594537124495, 378.5275384125996538, -187.0000000000000284 ) ) ;
#1303 =( LENGTH_UNIT ( ) NAMED_UNIT ( * ) SI_UNIT ( .MILLI., .METRE. ) );
#1304 = B_SPLINE_CURVE_WITH_KNOTS ( 'NONE', 3,
 ( #603, #1730, #12725, #2624, #5067, #6232 ),
 .UNSPECIFIED., .F., .F.,
 ( 4, 2, 4 ),
 ( 0.003841072314098362400, 0.005765657563962184665, 0.007690242813826007363 ),
 .UNSPECIFIED. ) ;
#1305 = ORIENTED_EDGE ( 'NONE', *, *, #9512, .F. ) ;
#1306 = FACE_OUTER_BOUND ( 'NONE', #4104, .T. ) ;
#1307 = VERTEX_POINT ( 'NONE', #5062 ) ;
#1308 = ORIENTED_EDGE ( 'NONE', *, *, #9612, .T. ) ;
#1309 = CARTESIAN_POINT ( 'NONE',  ( 6.725979247667765115, -3.622307570260320020, -6.470294263593358686 ) ) ;
#1310 =( REPRESENTATION_RELATIONSHIP ('NONE','NONE', #2822, #3781 ) REPRESENTATION_RELATIONSHIP_WITH_TRANSFORMATION ( #2437 )SHAPE_REPRESENTATION_RELATIONSHIP( ) );
#1311 = DIRECTION ( 'NONE',  ( 0.000000000000000000, 0.000000000000000000, 1.000000000000000000 ) ) ;
#1312 = EDGE_CURVE ( 'NONE', #9111, #7367, #10328, .T. ) ;
#1313 = DIRECTION ( 'NONE',  ( 0.000000000000000000, 0.000000000000000000, 1.000000000000000000 ) ) ;
#1314 = CYLINDRICAL_SURFACE ( 'NONE', #12760, 7.000000000000006217 ) ;
#1315 = EDGE_CURVE ( 'NONE', #1059, #2855, #4916, .T. ) ;
#1316 = DIRECTION ( 'NONE',  ( 9.304756960132325412E-16, 6.965275210156238168E-15, 1.000000000000000000 ) ) ;
#1317 = CARTESIAN_POINT ( 'NONE',  ( -31.74999999999995737, 0.000000000000000000, 2.500000000000000444 ) ) ;
#1318 = DIRECTION ( 'NONE',  ( 0.9578262852211513190, -0.2873478855663453846, 0.000000000000000000 ) ) ;
#1319 = VERTEX_POINT ( 'NONE', #10502 ) ;
#1320 = EDGE_CURVE ( 'NONE', #13064, #8019, #12802, .T. ) ;
#1321 = CARTESIAN_POINT ( 'NONE',  ( -2.000000000000000000, -6.429618962271402616, 0.000000000000000000 ) ) ;
#1322 = CARTESIAN_POINT ( 'NONE',  ( 0.000000000000000000, 0.5192545390863916310, 0.000000000000000000 ) ) ;
#1323 = CARTESIAN_POINT ( 'NONE',  ( 610.1812141201095301, 189.9029010627875493, 186.7093446292720387 ) ) ;
#1324 = VERTEX_POINT ( 'NONE', #8361 ) ;
#1326 = EDGE_CURVE ( 'NONE', #12898, #12523, #9621, .T. ) ;
#1325 = CYLINDRICAL_SURFACE ( 'NONE', #5457, 2.700000000000000178 ) ;
#1327 = VERTEX_POINT ( 'NONE', #3808 ) ;
#1328 = ORIENTED_EDGE ( 'NONE', *, *, #14247, .F. ) ;
#1329 = DIRECTION ( 'NONE',  ( 0.000000000000000000, -1.000000000000000000, 4.625616335171366110E-15 ) ) ;
#1330 = CARTESIAN_POINT ( 'NONE',  ( 6.452281807715718465, -2.898928808473054897, 5.021091983800450187 ) ) ;
#1331 = FACE_OUTER_BOUND ( 'NONE', #711, .T. ) ;
#1332 = CARTESIAN_POINT ( 'NONE',  ( 6.207671477328849718, -5.338259717474132415, -0.7538629453365324196 ) ) ;
#1333 = EDGE_LOOP ( 'NONE', ( #7672, #14460, #2611, #6334 ) ) ;
#1334 = ADVANCED_FACE ( 'NONE', ( #8292, #6291 ), #9555, .F. ) ;
#1335 = EDGE_CURVE ( 'NONE', #8820, #739, #4018, .T. ) ;
#1336 = CARTESIAN_POINT ( 'NONE',  ( 43.50000000000000711, 0.000000000000000000, 0.000000000000000000 ) ) ;
#1337 = CARTESIAN_POINT ( 'NONE',  ( 6.500000000000000000, -3.752776749732574135, -6.064240316920400886 ) ) ;
#1338 = CARTESIAN_POINT ( 'NONE',  ( 139.8040310085880833, 355.9707293956415697, 215.0000000000000000 ) ) ;
#1340 = EDGE_CURVE ( 'NONE', #10717, #8233, #11743, .T. ) ;
#1339 = DIRECTION ( 'NONE',  ( -0.9578262852211514300, 0.2873478855663453846, -9.382948195091500646E-16 ) ) ;
#1341 = ORIENTED_EDGE ( 'NONE', *, *, #6974, .F. ) ;
#1342 = ORIENTED_EDGE ( 'NONE', *, *, #9115, .F. ) ;
#1343 = CARTESIAN_POINT ( 'NONE',  ( 635.0000000000000000, 160.0000000000000284, 210.0000000000000000 ) ) ;
#1344 = LINE ( 'NONE', #4537, #4523 ) ;
#1345 = DIRECTION ( 'NONE',  ( 1.000000000000000000, 0.000000000000000000, 0.000000000000000000 ) ) ;
#1347 = EDGE_LOOP ( 'NONE', ( #7153, #12726, #8039, #8024 ) ) ;
#1346 = AXIS2_PLACEMENT_3D ( 'NONE', #14026, #11711, #4877 ) ;
#1348 = AXIS2_PLACEMENT_3D ( 'NONE', #1232, #5735, #94 ) ;
#1349 = ORIENTED_EDGE ( 'NONE', *, *, #7002, .F. ) ;
#1350 = CARTESIAN_POINT ( 'NONE',  ( -1.400000000000000133, 0.000000000000000000, 0.000000000000000000 ) ) ;
#1351 = CARTESIAN_POINT ( 'NONE',  ( 2.500000000000000000, 0.000000000000000000, 0.000000000000000000 ) ) ;
#1352 = CARTESIAN_POINT ( 'NONE',  ( 0.000000000000000000, 1.178949249685212974, -2.042000000000001148 ) ) ;
#1353 = CYLINDRICAL_SURFACE ( 'NONE', #2567, 4.799999999999968736 ) ;
#1354 = DIRECTION ( 'NONE',  ( -0.2873478855663441633, -0.9578262852211516520, 3.408579461568462910E-15 ) ) ;
#1355 = ORIENTED_EDGE ( 'NONE', *, *, #8452, .F. ) ;
#1356 = PLANE ( 'NONE',  #5436 ) ;
#1357 = ORIENTED_EDGE ( 'NONE', *, *, #9348, .F. ) ;
#1358 = EDGE_LOOP ( 'NONE', ( #5343, #14402, #10147, #3262 ) ) ;
#1359 = CARTESIAN_POINT ( 'NONE',  ( 6.092460485788117275, -1.005982284677391592, -5.000000000000000000 ) ) ;
#1360 = COLOUR_RGB ( '',0.8941176470588234615, 0.8941176470588234615, 0.8941176470588234615 ) ;
#1361 = VECTOR ( 'NONE', #4691, 1000.000000000000000 ) ;
#1362 = LINE ( 'NONE', #8222, #5207 ) ;
#1363 = PLANE ( 'NONE',  #4282 ) ;
#1364 = VERTEX_POINT ( 'NONE', #457 ) ;
#1365 = DIRECTION ( 'NONE',  ( 0.000000000000000000, 0.000000000000000000, -1.000000000000000000 ) ) ;
#1366 = DIRECTION ( 'NONE',  ( 1.000000000000000000, -0.000000000000000000, 0.000000000000000000 ) ) ;
#1367 = AXIS2_PLACEMENT_3D ( 'NONE', #672, #13093, #8512 ) ;
#1368 = CARTESIAN_POINT ( 'NONE',  ( 610.0000000000000000, 227.4403065089105951, -190.0000000000000000 ) ) ;
#1369 = DIRECTION ( 'NONE',  ( 0.000000000000000000, 0.000000000000000000, 1.000000000000000000 ) ) ;
#1370 =( NAMED_UNIT ( * ) PLANE_ANGLE_UNIT ( ) SI_UNIT ( $, .RADIAN. ) );
#1371 = VERTEX_POINT ( 'NONE', #13022 ) ;
#1372 = CARTESIAN_POINT ( 'NONE',  ( 0.000000000000000000, 0.000000000000000000, -6.800000000000000711 ) ) ;
#1373 = ORIENTED_EDGE ( 'NONE', *, *, #126, .F. ) ;
#1374 = ADVANCED_FACE ( 'NONE', ( #4987 ), #9704, .F. ) ;
#1375 = EDGE_CURVE ( 'NONE', #6946, #8693, #8587, .T. ) ;
#1376 = VERTEX_POINT ( 'NONE', #755 ) ;
#1377 = DIRECTION ( 'NONE',  ( -0.2873478855663534892, -0.9578262852211489875, 0.000000000000000000 ) ) ;
#1378 = VECTOR ( 'NONE', #1272, 1000.000000000000000 ) ;
#1379 = CARTESIAN_POINT ( 'NONE',  ( 642.3095993250867650, 158.0482295922596450, -210.0000000000000000 ) ) ;
#1380 = CARTESIAN_POINT ( 'NONE',  ( -4.078421086530219064, -3.990950201428956845, 0.000000000000000000 ) ) ;
#1381 = ORIENTED_EDGE ( 'NONE', *, *, #11454, .F. ) ;
#1382 = CARTESIAN_POINT ( 'NONE',  ( -1.604619215278546562E-14, -7.505553499465138501, -0.8000000000000003775 ) ) ;
#1383 = AXIS2_PLACEMENT_3D ( 'NONE', #10321, #13800, #5975 ) ;
#1384 = FACE_OUTER_BOUND ( 'NONE', #9975, .T. ) ;
#1385 = CARTESIAN_POINT ( 'NONE',  ( 459.3348797583642522, 272.6398425814014104, -210.0000000000000000 ) ) ;
#1386 = CARTESIAN_POINT ( 'NONE',  ( -4.726443845678993920E-16, -0.4883827417527498160, -4.999999999999999112 ) ) ;
#1387 = ORIENTED_EDGE ( 'NONE', *, *, #2488, .T. ) ;
#1388 = AXIS2_PLACEMENT_3D ( 'NONE', #11311, #6806, #2160 ) ;
#1389 = AXIS2_PLACEMENT_3D ( 'NONE', #10788, #8284, #2823 ) ;
#1390 = CARTESIAN_POINT ( 'NONE',  ( 611.4942090049451053, 232.4210031920605388, 190.0000000000000000 ) ) ;
#1391 = CARTESIAN_POINT ( 'NONE',  ( 0.2259792476677697226, -7.636022678937403718, -6.470294263593365791 ) ) ;
#1392 = CARTESIAN_POINT ( 'NONE',  ( 6.518095160332179283, 2.933089652807376435, -5.080260301816947432 ) ) ;
#1393 = CONTEXT_DEPENDENT_SHAPE_REPRESENTATION ( #13855, #13026 ) ;
#1394 = ORIENTED_EDGE ( 'NONE', *, *, #5211, .F. ) ;
#1395 = EDGE_CURVE ( 'NONE', #5257, #4953, #9858, .T. ) ;
#1396 = CARTESIAN_POINT ( 'NONE',  ( 4.197393957002303999, 7.772902908466098641E-14, -3.503767560748929810 ) ) ;
#1397 =( BOUNDED_SURFACE ( )  B_SPLINE_SURFACE ( 3, 2, ( 
 ( #9618, #13347, #4359 ),
 ( #6710, #2911, #7408 ),
 ( #9965, #11061, #9701 ),
 ( #11894, #4423, #8851 ),
 ( #7747, #14201, #4014 ),
 ( #8921, #8510, #12938 ) ),
 .UNSPECIFIED., .F., .F., .F. ) 
 B_SPLINE_SURFACE_WITH_KNOTS ( ( 4, 2, 4 ),
 ( 3, 3 ),
 ( 0.003190620565844220352, 0.007281897438794486706, 0.01137317431174475306 ),
 ( 0.000000000000000000, 1.000000000000000000 ),
 .UNSPECIFIED. ) 
 GEOMETRIC_REPRESENTATION_ITEM ( )  RATIONAL_B_SPLINE_SURFACE ( (
 ( 1.000000000000000000, 0.8047731410850402778, 1.000000000000000000),
 ( 1.000000000000000000, 0.8125552299142427826, 1.000000000000000000),
 ( 1.000000000000000000, 0.8191520442908248878, 1.000000000000000000),
 ( 1.000000000000000000, 0.8191520442871482732, 1.000000000000000000),
 ( 1.000000000000000000, 0.8125552299170040182, 1.000000000000000000),
 ( 1.000000000000000000, 0.8047731410850399447, 1.000000000000000000) ) ) 
 REPRESENTATION_ITEM ( '' )  SURFACE ( )  );
#1398 = ORIENTED_EDGE ( 'NONE', *, *, #3960, .T. ) ;
#1399 = ORIENTED_EDGE ( 'NONE', *, *, #2767, .F. ) ;
#1400 = LINE ( 'NONE', #5761, #14573 ) ;
#1401 = CARTESIAN_POINT ( 'NONE',  ( 0.3572655899081578768, -4.618802153516999631, -3.329030144205522754E-16 ) ) ;
#1402 = DIRECTION ( 'NONE',  ( -0.000000000000000000, -0.000000000000000000, -1.000000000000000000 ) ) ;
#1403 = AXIS2_PLACEMENT_3D ( 'NONE', #13360, #13522, #12174 ) ;
#1404 = EDGE_CURVE ( 'NONE', #5419, #13232, #3263, .T. ) ;
#1405 = AXIS2_PLACEMENT_3D ( 'NONE', #5448, #7508, #10976 ) ;
#1406 = CARTESIAN_POINT ( 'NONE',  ( -2.267930716273388369E-15, 0.3911686820828841893, 3.999999999999995559 ) ) ;
#1407 = DIRECTION ( 'NONE',  ( -0.000000000000000000, -0.000000000000000000, 1.000000000000000000 ) ) ;
#1408 = ORIENTED_EDGE ( 'NONE', *, *, #1824, .F. ) ;
#1409 = AXIS2_PLACEMENT_3D ( 'NONE', #13307, #4316, #5280 ) ;
#1410 = CARTESIAN_POINT ( 'NONE',  ( -8.505790995054894665, 376.6597771564184427, -184.8000000000000398 ) ) ;
#1411 = DIRECTION ( 'NONE',  ( 0.000000000000000000, -1.000000000000000000, 0.000000000000000000 ) ) ;
#1412 = DIRECTION ( 'NONE',  ( 0.000000000000000000, 0.000000000000000000, 1.000000000000000000 ) ) ;
#1413 = EDGE_CURVE ( 'NONE', #2369, #1324, #2296, .T. ) ;
#1414 = VECTOR ( 'NONE', #13789, 1000.000000000000114 ) ;
#1415 = CARTESIAN_POINT ( 'NONE',  ( 639.0000000000000000, 156.0000000000000000, -233.5000000000000000 ) ) ;
#1416 = AXIS2_PLACEMENT_3D ( 'NONE', #12274, #4328, #9037 ) ;
#1417 = ORIENTED_EDGE ( 'NONE', *, *, #6202, .F. ) ;
#1418 = ORIENTED_EDGE ( 'NONE', *, *, #3188, .T. ) ;
#1419 = DIRECTION ( 'NONE',  ( 0.000000000000000000, 0.000000000000000000, 1.000000000000000000 ) ) ;
#1420 = CARTESIAN_POINT ( 'NONE',  ( 610.0000000000002274, 185.6790804732676747, 8.443403382996446544E-13 ) ) ;
#1421 =( REPRESENTATION_RELATIONSHIP ('NONE','NONE', #2822, #1780 ) REPRESENTATION_RELATIONSHIP_WITH_TRANSFORMATION ( #6475 )SHAPE_REPRESENTATION_RELATIONSHIP( ) );
#1422 = CARTESIAN_POINT ( 'NONE',  ( 6.362374563307939823, 3.415000007733389076, 4.302769906042884784 ) ) ;
#1423 = VECTOR ( 'NONE', #7760, 1000.000000000000000 ) ;
#1424 = AXIS2_PLACEMENT_3D ( 'NONE', #10126, #11383, #66 ) ;
#1425 = EDGE_CURVE ( 'NONE', #10194, #525, #4233, .T. ) ;
#1426 = AXIS2_PLACEMENT_3D ( 'NONE', #3378, #13189, #7877 ) ;
#1427 = ORIENTED_EDGE ( 'NONE', *, *, #7911, .T. ) ;
#1428 = EDGE_CURVE ( 'NONE', #12947, #2635, #10045, .T. ) ;
#1429 = VECTOR ( 'NONE', #9770, 1000.000000000000000 ) ;
#1430 = PRODUCT_RELATED_PRODUCT_CATEGORY ( 'part', '', ( #12531 ) ) ;
#1431 = EDGE_LOOP ( 'NONE', ( #8093, #11408, #3433, #2468 ) ) ;
#1432 = DIRECTION ( 'NONE',  ( 0.000000000000000000, -1.000000000000000000, 0.000000000000000000 ) ) ;
#1433 = DIRECTION ( 'NONE',  ( 0.000000000000000000, 0.000000000000000000, 1.000000000000000000 ) ) ;
#1434 = DIRECTION ( 'NONE',  ( -0.000000000000000000, -0.000000000000000000, 1.000000000000000000 ) ) ;
#1435 = DIRECTION ( 'NONE',  ( 0.000000000000000000, 0.000000000000000000, 1.000000000000000000 ) ) ;
#1436 = SURFACE_STYLE_FILL_AREA ( #12870 ) ;
#1437 = AXIS2_PLACEMENT_3D ( 'NONE', #800, #13135, #14530 ) ;
#1438 = ORIENTED_EDGE ( 'NONE', *, *, #12056, .T. ) ;
#1439 = AXIS2_PLACEMENT_3D ( 'NONE', #6477, #11186, #12285 ) ;
#1440 = CARTESIAN_POINT ( 'NONE',  ( 0.000000000000000000, 0.000000000000000000, 0.000000000000000000 ) ) ;
#1441 = ORIENTED_EDGE ( 'NONE', *, *, #13691, .T. ) ;
#1442 = EDGE_LOOP ( 'NONE', ( #2693, #5441, #7947, #6102 ) ) ;
#1443 = CARTESIAN_POINT ( 'NONE',  ( 6.095462721915160920, 1.047438013716504246, -5.000000000000000000 ) ) ;
#1444 = VECTOR ( 'NONE', #262, 1000.000000000000000 ) ;
#1445 =( GEOMETRIC_REPRESENTATION_CONTEXT ( 3 ) GLOBAL_UNCERTAINTY_ASSIGNED_CONTEXT ( ( #5319 ) ) GLOBAL_UNIT_ASSIGNED_CONTEXT ( ( #1820, #9204, #5737 ) ) REPRESENTATION_CONTEXT ( 'NONE', 'WORKASPACE' ) );
#1446 = DIRECTION ( 'NONE',  ( 0.000000000000000000, 0.000000000000000000, 1.000000000000000000 ) ) ;
#1447 = AXIS2_PLACEMENT_3D ( 'NONE', #13346, #3239, #1833 ) ;
#1448 = CIRCLE ( 'NONE', #1920, 4.199999999999926459 ) ;
#1449 = DIRECTION ( 'NONE',  ( -0.000000000000000000, -0.000000000000000000, 1.000000000000000000 ) ) ;
#1450 = EDGE_LOOP ( 'NONE', ( #12786, #4351, #13329, #7081 ) ) ;
#1451 = DIRECTION ( 'NONE',  ( 1.000000000000000000, 0.000000000000000000, 0.000000000000000000 ) ) ;
#1452 = DIRECTION ( 'NONE',  ( -0.2873478855663461062, -0.9578262852211510969, 0.000000000000000000 ) ) ;
#1453 = STYLED_ITEM ( 'NONE', ( #1805 ), #3692 ) ;
#1454 = CARTESIAN_POINT ( 'NONE',  ( 229.2257385731836621, 308.4724102386185223, -182.8000000000004945 ) ) ;
#1455 = DIRECTION ( 'NONE',  ( 0.000000000000000000, 0.000000000000000000, 1.000000000000000000 ) ) ;
#1456 = VERTEX_POINT ( 'NONE', #9912 ) ;
#1457 = EDGE_CURVE ( 'NONE', #9718, #6337, #5337, .T. ) ;
#1458 = DIRECTION ( 'NONE',  ( 1.000000000000000000, -0.000000000000000000, -0.000000000000000000 ) ) ;
#1459 = EDGE_CURVE ( 'NONE', #10035, #14129, #8436, .T. ) ;
#1460 = EDGE_LOOP ( 'NONE', ( #10013, #14172, #4888, #11929 ) ) ;
#1461 = CIRCLE ( 'NONE', #5465, 4.199999999999981526 ) ;
#1462 = ADVANCED_FACE ( 'NONE', ( #13237 ), #971, .F. ) ;
#1463 = ORIENTED_EDGE ( 'NONE', *, *, #9445, .F. ) ;
#1464 = CARTESIAN_POINT ( 'NONE',  ( 6.781345014477444089, -3.590342129888862921, -6.122077150241852728 ) ) ;
#1465 = AXIS2_PLACEMENT_3D ( 'NONE', #11727, #6141, #4969 ) ;
#1466 = CARTESIAN_POINT ( 'NONE',  ( 0.1739375980333730809, 5.301268757141563093, -0.8179331680533001858 ) ) ;
#1467 = DIRECTION ( 'NONE',  ( -0.4113766427172327877, 0.9114654452181378819, 0.000000000000000000 ) ) ;
#1468 = AXIS2_PLACEMENT_3D ( 'NONE', #8105, #13796, #9136 ) ;
#1469 = ORIENTED_EDGE ( 'NONE', *, *, #13140, .F. ) ;
#1470 = CARTESIAN_POINT ( 'NONE',  ( 706.6446721788142895, 159.8177707722969672, 177.6000000000001933 ) ) ;
#1471 = EDGE_CURVE ( 'NONE', #8142, #6053, #12201, .T. ) ;
#1472 = CARTESIAN_POINT ( 'NONE',  ( 8.500000000000000000, 0.000000000000000000, 0.000000000000000000 ) ) ;
#1473 = FACE_OUTER_BOUND ( 'NONE', #9867, .T. ) ;
#1474 = LINE ( 'NONE', #3622, #8347 ) ;
#1475 = EDGE_LOOP ( 'NONE', ( #7036, #7021, #298, #13292 ) ) ;
#1476 = PRODUCT_DEFINITION_FORMATION_WITH_SPECIFIED_SOURCE ( 'ANY', '', #5136, .NOT_KNOWN. ) ;
#1477 = DIRECTION ( 'NONE',  ( 0.000000000000000000, 0.000000000000000000, 1.000000000000000000 ) ) ;
#1478 = FACE_OUTER_BOUND ( 'NONE', #1563, .T. ) ;
#1479 = ORIENTED_EDGE ( 'NONE', *, *, #764, .F. ) ;
#1480 = DIRECTION ( 'NONE',  ( 1.000000000000000000, 0.000000000000000000, 0.000000000000000000 ) ) ;
#1481 = ORIENTED_EDGE ( 'NONE', *, *, #4412, .T. ) ;
#1482 = ORIENTED_EDGE ( 'NONE', *, *, #8935, .T. ) ;
#1483 = DIRECTION ( 'NONE',  ( 0.000000000000000000, 0.000000000000000000, 1.000000000000000000 ) ) ;
#1484 = ADVANCED_FACE ( 'NONE', ( #1861 ), #6588, .F. ) ;
#1485 = FACE_OUTER_BOUND ( 'NONE', #946, .T. ) ;
#1486 = AXIS2_PLACEMENT_3D ( 'NONE', #5292, #3150, #10961 ) ;
#1487 = LINE ( 'NONE', #1623, #5551 ) ;
#1488 = ORIENTED_EDGE ( 'NONE', *, *, #5661, .F. ) ;
#1489 =( BOUNDED_SURFACE ( )  B_SPLINE_SURFACE ( 3, 2, ( 
 ( #9088, #4599, #13588 ),
 ( #4442, #11378, #4753 ),
 ( #10202, #6876, #5619 ),
 ( #7975, #6725, #1268 ),
 ( #1332, #5547, #11298 ),
 ( #10119, #2368, #3478 ) ),
 .UNSPECIFIED., .F., .F., .F. ) 
 B_SPLINE_SURFACE_WITH_KNOTS ( ( 4, 2, 4 ),
 ( 3, 3 ),
 ( 0.02367865728600892367, 0.02663179453327098323, 0.02958493178053304279 ),
 ( 0.000000000000000000, 1.000000000000000000 ),
 .UNSPECIFIED. ) 
 GEOMETRIC_REPRESENTATION_ITEM ( )  RATIONAL_B_SPLINE_SURFACE ( (
 ( 1.000000000000000000, 0.8047781103519396906, 1.000000000000000000),
 ( 1.000000000000000000, 0.8123785825973208752, 1.000000000000000000),
 ( 1.000000000000000000, 0.8190671539297160741, 1.000000000000000000),
 ( 1.000000000000000000, 0.8192352255325974220, 1.000000000000000000),
 ( 1.000000000000000000, 0.8126129676842738236, 1.000000000000000000),
 ( 1.000000000000000000, 0.8047712537969737845, 1.000000000000000000) ) ) 
 REPRESENTATION_ITEM ( '' )  SURFACE ( )  );
#1490 = DIRECTION ( 'NONE',  ( 1.000000000000000000, 0.000000000000000000, 0.000000000000000000 ) ) ;
#1491 = CARTESIAN_POINT ( 'NONE',  ( -1.144235203016679359, -3.958177651039096911, -0.09382832055446428676 ) ) ;
#1492 = DIRECTION ( 'NONE',  ( -1.000000000000000000, 0.000000000000000000, 0.000000000000000000 ) ) ;
#1493 = DIRECTION ( 'NONE',  ( -0.000000000000000000, -1.000000000000000000, -0.000000000000000000 ) ) ;
#1494 = ORIENTED_EDGE ( 'NONE', *, *, #8612, .F. ) ;
#1495 = ORIENTED_EDGE ( 'NONE', *, *, #12220, .T. ) ;
#1496 = CARTESIAN_POINT ( 'NONE',  ( 451.3035746174797396, 294.6698471414878782, -210.0000000000000000 ) ) ;
#1497 = CARTESIAN_POINT ( 'NONE',  ( -2.354826896168714434, -6.962563485461402024, -1.000000000000000000 ) ) ;
#1498 = LINE ( 'NONE', #10496, #8925 ) ;
#1499 = EDGE_CURVE ( 'NONE', #902, #7765, #3348, .T. ) ;
#1500 = ORIENTED_EDGE ( 'NONE', *, *, #7365, .T. ) ;
#1501 = LINE ( 'NONE', #12864, #2181 ) ;
#1502 = CARTESIAN_POINT ( 'NONE',  ( 610.0429133068968213, 190.7986032820865319, -186.9697000000000173 ) ) ;
#1503 = DIRECTION ( 'NONE',  ( 0.2873478855663453846, 0.9578262852211513190, 0.000000000000000000 ) ) ;
#1504 = EDGE_CURVE ( 'NONE', #6153, #7939, #11006, .T. ) ;
#1505 = DIRECTION ( 'NONE',  ( 0.000000000000000000, -0.5000000000000009992, -0.8660254037844380415 ) ) ;
#1506 = CARTESIAN_POINT ( 'NONE',  ( 5.686050877451574337, -5.768780236673276995, 0.000000000000000000 ) ) ;
#1507 = CARTESIAN_POINT ( 'NONE',  ( 137.1540310085880776, 355.9707293956415697, -210.0000000000000000 ) ) ;
#1508 = APPLICATION_CONTEXT ( 'automotive_design' ) ;
#1509 = ORIENTED_EDGE ( 'NONE', *, *, #10325, .F. ) ;
#1510 = EDGE_CURVE ( 'NONE', #6705, #5856, #11501, .T. ) ;
#1511 = CARTESIAN_POINT ( 'NONE',  ( 2.712762565639649015, -3.052587955997662306, -3.430618716626630871 ) ) ;
#1512 = ORIENTED_EDGE ( 'NONE', *, *, #4932, .T. ) ;
#1513 = VERTEX_POINT ( 'NONE', #10945 ) ;
#1514 = CYLINDRICAL_SURFACE ( 'NONE', #14409, 2.649999999999985700 ) ;
#1515 = EDGE_CURVE ( 'NONE', #12673, #2108, #9837, .T. ) ;
#1516 = LINE ( 'NONE', #9412, #9511 ) ;
#1517 = CARTESIAN_POINT ( 'NONE',  ( 2.500000000000000000, 2.357898499370431722, -2.818925648462311528E-15 ) ) ;
#1518 = DIRECTION ( 'NONE',  ( 0.000000000000000000, 0.000000000000000000, 1.000000000000000000 ) ) ;
#1519 = ORIENTED_EDGE ( 'NONE', *, *, #9574, .F. ) ;
#1520 = LINE ( 'NONE', #386, #8999 ) ;
#1521 = CARTESIAN_POINT ( 'NONE',  ( 6.500000000000576428, -2.723981882618385697, -6.224051986860747121 ) ) ;
#1522 = CARTESIAN_POINT ( 'NONE',  ( -6.837824896291514243, 3.947820044545427454, -6.564402953523716278 ) ) ;
#1523 = DIRECTION ( 'NONE',  ( -0.000000000000000000, -0.000000000000000000, -1.000000000000000000 ) ) ;
#1524 = ORIENTED_EDGE ( 'NONE', *, *, #7166, .T. ) ;
#1525 = EDGE_CURVE ( 'NONE', #2008, #2622, #11004, .T. ) ;
#1526 = EDGE_CURVE ( 'NONE', #10480, #13545, #3745, .T. ) ;
#1527 = DIRECTION ( 'NONE',  ( 1.000000000000000000, 0.000000000000000000, -0.000000000000000000 ) ) ;
#1528 = ORIENTED_EDGE ( 'NONE', *, *, #4356, .F. ) ;
#1529 = CARTESIAN_POINT ( 'NONE',  ( 4.154306624730864428, 2.398490048084778170, -3.721999068284300272 ) ) ;
#1530 = CARTESIAN_POINT ( 'NONE',  ( 650.0000000000000000, 175.0000000000000568, -210.0000000000000000 ) ) ;
#1531 = CARTESIAN_POINT ( 'NONE',  ( 455.5035746174796714, 294.6698471414878782, 190.0000000000000000 ) ) ;
#1532 = EDGE_CURVE ( 'NONE', #6611, #818, #11041, .T. ) ;
#1533 = ORIENTED_EDGE ( 'NONE', *, *, #1248, .F. ) ;
#1534 = CARTESIAN_POINT ( 'NONE',  ( 609.7043258424479291, 187.8603929224640581, 188.9582675804705332 ) ) ;
#1535 = CARTESIAN_POINT ( 'NONE',  ( 726.1975094929949819, 167.5243180396262801, -149.9999999999986358 ) ) ;
#1536 = CARTESIAN_POINT ( 'NONE',  ( 0.4465819873851989974, -2.886751345948121106, 4.999999999999999112 ) ) ;
#1537 = CARTESIAN_POINT ( 'NONE',  ( 0.5636800770130377947, 4.293361309317166530, -3.531542292954102713 ) ) ;
#1538 = VERTEX_POINT ( 'NONE', #11162 ) ;
#1539 = SURFACE_STYLE_FILL_AREA ( #11789 ) ;
#1540 = CARTESIAN_POINT ( 'NONE',  ( 6.244889965166094292, 4.918546365148221078, -1.691415889817840412 ) ) ;
#1541 = EDGE_LOOP ( 'NONE', ( #3116, #12222, #10523, #7416 ) ) ;
#1542 = CARTESIAN_POINT ( 'NONE',  ( 2.499999999999999556, 0.000000000000000000, 3.469446951953614189E-15 ) ) ;
#1543 = ORIENTED_EDGE ( 'NONE', *, *, #8563, .F. ) ;
#1544 = VERTEX_POINT ( 'NONE', #1038 ) ;
#1545 = DIRECTION ( 'NONE',  ( 1.000000000000000000, 0.000000000000000000, 0.000000000000000000 ) ) ;
#1546 = DIRECTION ( 'NONE',  ( -0.9578262852211507639, 0.2873478855663477716, -0.000000000000000000 ) ) ;
#1547 = CARTESIAN_POINT ( 'NONE',  ( -6.500000000000000888, -3.752776749732573247, -6.177802698399960768 ) ) ;
#1548 = PLANE ( 'NONE',  #11567 ) ;
#1549 = DIRECTION ( 'NONE',  ( -0.000000000000000000, 0.5000000000000014433, 0.8660254037844378194 ) ) ;
#1550 = CARTESIAN_POINT ( 'NONE',  ( 152.8304684875957378, 364.5911659626319192, 190.0000000000000000 ) ) ;
#1551 = ORIENTED_EDGE ( 'NONE', *, *, #7851, .T. ) ;
#1552 = LINE ( 'NONE', #10711, #12900 ) ;
#1553 = FACE_BOUND ( 'NONE', #8777, .T. ) ;
#1554 = DIRECTION ( 'NONE',  ( 1.000000000000000000, 0.000000000000000000, 0.000000000000000000 ) ) ;
#1555 = FACE_OUTER_BOUND ( 'NONE', #14485, .T. ) ;
#1556 = ORIENTED_EDGE ( 'NONE', *, *, #3833, .F. ) ;
#1557 = ORIENTED_EDGE ( 'NONE', *, *, #3933, .T. ) ;
#1558 = DIRECTION ( 'NONE',  ( 0.000000000000000000, 0.000000000000000000, 1.000000000000000000 ) ) ;
#1559 = DIRECTION ( 'NONE',  ( -1.000000000000000000, -0.000000000000000000, -0.000000000000000000 ) ) ;
#1560 = ADVANCED_FACE ( 'NONE', ( #5549 ), #14553, .F. ) ;
#1561 = CARTESIAN_POINT ( 'NONE',  ( 610.0000000000000000, 227.4403065089105951, -210.0000000000000000 ) ) ;
#1562 = DIRECTION ( 'NONE',  ( 0.000000000000000000, 0.000000000000000000, -1.000000000000000000 ) ) ;
#1563 = EDGE_LOOP ( 'NONE', ( #9615, #3354, #5095, #1269 ) ) ;
#1564 = CARTESIAN_POINT ( 'NONE',  ( -8.505790995055050985, 376.6597771564184995, 184.8000000000000398 ) ) ;
#1565 = CARTESIAN_POINT ( 'NONE',  ( 6.495567275914606142, -2.917443832165063533, -5.053160945538327731 ) ) ;
#1566 = LINE ( 'NONE', #9179, #4728 ) ;
#1567 = CARTESIAN_POINT ( 'NONE',  ( 629.0000000000000000, 166.0000000000000284, -187.5000000000000000 ) ) ;
#1568 = CARTESIAN_POINT ( 'NONE',  ( 2.100000000000000089, 0.000000000000000000, -5.000000000000000000 ) ) ;
#1569 = FILL_AREA_STYLE_COLOUR ( '', #13720 ) ;
#1570 = EDGE_LOOP ( 'NONE', ( #3192, #9625, #14307, #7227 ) ) ;
#1571 = CARTESIAN_POINT ( 'NONE',  ( 4.999999999999997335, 0.000000000000000000, 4.250000000000000000 ) ) ;
#1572 = ORIENTED_EDGE ( 'NONE', *, *, #12129, .F. ) ;
#1573 = VERTEX_POINT ( 'NONE', #7852 ) ;
#1574 = AXIS2_PLACEMENT_3D ( 'NONE', #7528, #7611, #4142 ) ;
#1575 = LINE ( 'NONE', #4915, #1681 ) ;
#1576 = EDGE_CURVE ( 'NONE', #4895, #4552, #10097, .T. ) ;
#1577 = EDGE_CURVE ( 'NONE', #12373, #10093, #9834, .T. ) ;
#1578 = CONICAL_SURFACE ( 'NONE', #7238, 4.000000000000000000, 1.047197551196600296 ) ;
#1579 = DIRECTION ( 'NONE',  ( 1.000000000000000000, 0.000000000000000000, 0.000000000000000000 ) ) ;
#1580 = CARTESIAN_POINT ( 'NONE',  ( 0.000000000000000000, 0.000000000000000000, -1.000000000000000000 ) ) ;
#1582 = EDGE_CURVE ( 'NONE', #14148, #11328, #2371, .T. ) ;
#1581 = LINE ( 'NONE', #6240, #6770 ) ;
#1583 = ORIENTED_EDGE ( 'NONE', *, *, #617, .F. ) ;
#1584 = CARTESIAN_POINT ( 'NONE',  ( 611.4942090049448780, 232.4210031920598283, 184.7999999999999829 ) ) ;
#1585 = DIRECTION ( 'NONE',  ( 0.2873478855663471054, 0.9578262852211508749, 1.632680918566126195E-14 ) ) ;
#1586 = EDGE_CURVE ( 'NONE', #4487, #4582, #462, .T. ) ;
#1587 = CARTESIAN_POINT ( 'NONE',  ( -6.500000000000000000, 3.752776749732564809, -8.000000000000000000 ) ) ;
#1588 = SURFACE_STYLE_USAGE ( .BOTH. , #3896 ) ;
#1589 = ORIENTED_EDGE ( 'NONE', *, *, #5597, .T. ) ;
#1590 = VECTOR ( 'NONE', #9416, 1000.000000000000000 ) ;
#1591 = LINE ( 'NONE', #10682, #4472 ) ;
#1592 = VECTOR ( 'NONE', #10818, 1000.000000000000114 ) ;
#1593 = EDGE_LOOP ( 'NONE', ( #7270, #9100, #14362 ) ) ;
#1594 = LINE ( 'NONE', #9653, #10816 ) ;
#1595 = DIRECTION ( 'NONE',  ( 0.000000000000000000, 0.000000000000000000, -1.000000000000000000 ) ) ;
#1596 = DIRECTION ( 'NONE',  ( -0.000000000000000000, -0.000000000000000000, -1.000000000000000000 ) ) ;
#1597 = AXIS2_PLACEMENT_3D ( 'NONE', #8501, #1930, #12858 ) ;
#1598 = ADVANCED_FACE ( 'NONE', ( #13528 ), #2447, .F. ) ;
#1599 = AXIS2_PLACEMENT_3D ( 'NONE', #10361, #10440, #2618 ) ;
#1600 = ORIENTED_EDGE ( 'NONE', *, *, #10084, .F. ) ;
#1601 = CARTESIAN_POINT ( 'NONE',  ( 609.7412162373094588, 188.4357741873886880, 189.3699028110927429 ) ) ;
#1602 = EDGE_CURVE ( 'NONE', #9849, #7148, #142, .T. ) ;
#1603 = PRODUCT_DEFINITION ( 'UNKNOWN', '', #270, #5912 ) ;
#1604 = CYLINDRICAL_SURFACE ( 'NONE', #12074, 2.499999999999946709 ) ;
#1605 = CARTESIAN_POINT ( 'NONE',  ( 5.686050877451574337, -5.768780236673276995, -1.000000000000000000 ) ) ;
#1606 = LINE ( 'NONE', #4809, #9482 ) ;
#1607 = ORIENTED_EDGE ( 'NONE', *, *, #3104, .F. ) ;
#1608 = LINE ( 'NONE', #6260, #8458 ) ;
#1609 = DIRECTION ( 'NONE',  ( 0.000000000000000000, 0.000000000000000000, 1.000000000000000000 ) ) ;
#1610 = EDGE_LOOP ( 'NONE', ( #4110, #12927, #11663, #6845 ) ) ;
#1611 = MECHANICAL_DESIGN_GEOMETRIC_PRESENTATION_REPRESENTATION (  '', ( #13870 ), #418 ) ;
#1612 = DIRECTION ( 'NONE',  ( -0.000000000000000000, -0.000000000000000000, -1.000000000000000000 ) ) ;
#1613 = VECTOR ( 'NONE', #7698, 1000.000000000000227 ) ;
#1614 = AXIS2_PLACEMENT_3D ( 'NONE', #5274, #13367, #12115 ) ;
#1615 = EDGE_LOOP ( 'NONE', ( #3200, #3091, #4348, #1810 ) ) ;
#1616 = ORIENTED_EDGE ( 'NONE', *, *, #10512, .F. ) ;
#1617 = DIRECTION ( 'NONE',  ( -1.000000000000000000, -0.000000000000000000, -0.000000000000000000 ) ) ;
#1618 = FACE_BOUND ( 'NONE', #5385, .T. ) ;
#1619 = FACE_OUTER_BOUND ( 'NONE', #2576, .T. ) ;
#1620 = DIRECTION ( 'NONE',  ( -1.000000000000000000, -0.000000000000000000, -0.000000000000000000 ) ) ;
#1621 = CIRCLE ( 'NONE', #4452, 7.500000000000062172 ) ;
#1622 = VECTOR ( 'NONE', #4145, 1000.000000000000000 ) ;
#1623 = CARTESIAN_POINT ( 'NONE',  ( 590.0000000000000000, 212.5596934910894333, -210.0000000000000000 ) ) ;
#1624 = ORIENTED_EDGE ( 'NONE', *, *, #13598, .T. ) ;
#1625 = DIRECTION ( 'NONE',  ( 0.000000000000000000, 0.000000000000000000, -1.000000000000000000 ) ) ;
#1626 = DIRECTION ( 'NONE',  ( 1.000000000000000000, -3.469446951953611033E-15, 0.000000000000000000 ) ) ;
#1627 = DIRECTION ( 'NONE',  ( 1.000000000000000000, 0.000000000000000000, 0.000000000000000000 ) ) ;
#1628 = VECTOR ( 'NONE', #7598, 1000.000000000000114 ) ;
#1629 = DIRECTION ( 'NONE',  ( 1.000000000000000000, 0.000000000000000000, 0.000000000000000000 ) ) ;
#1630 = VERTEX_POINT ( 'NONE', #1107 ) ;
#1631 = ORIENTED_EDGE ( 'NONE', *, *, #2654, .T. ) ;
#1632 = CYLINDRICAL_SURFACE ( 'NONE', #9383, 5.525000000000000355 ) ;
#1633 = FACE_BOUND ( 'NONE', #13457, .T. ) ;
#1634 = B_SPLINE_CURVE_WITH_KNOTS ( 'NONE', 3,
 ( #8242, #12755, #2648, #7146, #405 ),
 .UNSPECIFIED., .F., .F.,
 ( 4, 1, 4 ),
 ( 0.000000000000000000, 0.002309401076758505356, 0.004618802153517010713 ),
 .UNSPECIFIED. ) ;
#1635 = AXIS2_PLACEMENT_3D ( 'NONE', #14546, #8800, #9017 ) ;
#1636 = ADVANCED_FACE ( 'NONE', ( #2286 ), #6541, .T. ) ;
#1637 = AXIS2_PLACEMENT_3D ( 'NONE', #10873, #6285, #749 ) ;
#1638 = PLANE ( 'NONE',  #4224 ) ;
#1639 = CYLINDRICAL_SURFACE ( 'NONE', #1637, 2.500000000000000444 ) ;
#1640 = VECTOR ( 'NONE', #9507, 1000.000000000000114 ) ;
#1641 = EDGE_LOOP ( 'NONE', ( #4198, #14567, #10049, #8130 ) ) ;
#1642 = DIRECTION ( 'NONE',  ( -1.000000000000000000, 0.000000000000000000, 0.000000000000000000 ) ) ;
#1643 = CARTESIAN_POINT ( 'NONE',  ( 610.8707502976318438, 188.5815814653741427, -184.8000000000000682 ) ) ;
#1644 = CARTESIAN_POINT ( 'NONE',  ( 0.000000000000000000, 0.000000000000000000, 0.000000000000000000 ) ) ;
#1645 = AXIS2_PLACEMENT_3D ( 'NONE', #13635, #178, #7063 ) ;
#1646 = AXIS2_PLACEMENT_3D ( 'NONE', #12884, #2769, #9346 ) ;
#1647 = EDGE_CURVE ( 'NONE', #11118, #10957, #11227, .T. ) ;
#1648 = DIRECTION ( 'NONE',  ( -0.2873478855663427756, -0.9578262852211522071, 0.000000000000000000 ) ) ;
#1649 = LINE ( 'NONE', #13910, #10791 ) ;
#1650 =( NAMED_UNIT ( * ) SI_UNIT ( $, .STERADIAN. ) SOLID_ANGLE_UNIT ( ) );
#1651 =( NAMED_UNIT ( * ) PLANE_ANGLE_UNIT ( ) SI_UNIT ( $, .RADIAN. ) );
#1652 = VERTEX_POINT ( 'NONE', #3566 ) ;
#1653 = CARTESIAN_POINT ( 'NONE',  ( 3.436319922986518449, -2.634841920959471562, -3.531542292954761741 ) ) ;
#1654 = ORIENTED_EDGE ( 'NONE', *, *, #6129, .F. ) ;
#1655 = ORIENTED_EDGE ( 'NONE', *, *, #11956, .T. ) ;
#1656 = CIRCLE ( 'NONE', #9902, 5.000000000000004441 ) ;
#1657 = PLANE ( 'NONE',  #7337 ) ;
#1658 = AXIS2_PLACEMENT_3D ( 'NONE', #6165, #10667, #463 ) ;
#1659 = AXIS2_PLACEMENT_3D ( 'NONE', #12812, #3819, #545 ) ;
#1660 = VECTOR ( 'NONE', #1433, 1000.000000000000000 ) ;
#1661 = CARTESIAN_POINT ( 'NONE',  ( 604.3113219698392413, -181.2933965909535914, -182.7999999999974250 ) ) ;
#1662 = LINE ( 'NONE', #11756, #2513 ) ;
#1663 = CARTESIAN_POINT ( 'NONE',  ( 8.500000000000000000, 9.800365875394399578E-16, -7.900000000000002132 ) ) ;
#1664 = AXIS2_PLACEMENT_3D ( 'NONE', #9751, #13284, #7679 ) ;
#1665 = ORIENTED_EDGE ( 'NONE', *, *, #8262, .F. ) ;
#1666 = DIRECTION ( 'NONE',  ( 0.2873478855663452736, 0.9578262852211513190, -3.491481338843133355E-15 ) ) ;
#1667 = EDGE_CURVE ( 'NONE', #3851, #9996, #1153, .T. ) ;
#1668 = CARTESIAN_POINT ( 'NONE',  ( 6.499999999999398703, -1.392325603688425284, -6.058577540042510812 ) ) ;
#1669 = AXIS2_PLACEMENT_3D ( 'NONE', #12242, #5758, #10259 ) ;
#1670 = FACE_OUTER_BOUND ( 'NONE', #4542, .T. ) ;
#1671 = PLANE ( 'NONE',  #5032 ) ;
#1672 =( NAMED_UNIT ( * ) PLANE_ANGLE_UNIT ( ) SI_UNIT ( $, .RADIAN. ) );
#1673 = ORIENTED_EDGE ( 'NONE', *, *, #4100, .F. ) ;
#1674 = AXIS2_PLACEMENT_3D ( 'NONE', #6769, #13345, #7891 ) ;
#1675 = STYLED_ITEM ( 'NONE', ( #7137 ), #11811 ) ;
#1676 = CARTESIAN_POINT ( 'NONE',  ( 1.049032378833991030, 6.899894373156697291, -0.3607371497494544221 ) ) ;
#1677 = CARTESIAN_POINT ( 'NONE',  ( 6.420058897733097680, 2.891482565094590562, -5.008194711943424693 ) ) ;
#1678 = ORIENTED_EDGE ( 'NONE', *, *, #9942, .T. ) ;
#1680 = DIRECTION ( 'NONE',  ( -1.000000000000000000, 5.337610695313498298E-15, 0.000000000000000000 ) ) ;
#1679 = CIRCLE ( 'NONE', #9928, 2.649999999999985700 ) ;
#1681 = VECTOR ( 'NONE', #467, 1000.000000000000114 ) ;
#1682 = DIRECTION ( 'NONE',  ( 0.000000000000000000, 0.000000000000000000, 1.000000000000000000 ) ) ;
#1683 = CARTESIAN_POINT ( 'NONE',  ( 0.1481481481481481122, -4.797713218419819903, -1.000000000000000000 ) ) ;
#1684 =( GEOMETRIC_REPRESENTATION_CONTEXT ( 3 ) GLOBAL_UNCERTAINTY_ASSIGNED_CONTEXT ( ( #4141 ) ) GLOBAL_UNIT_ASSIGNED_CONTEXT ( ( #7997, #12353, #5509 ) ) REPRESENTATION_CONTEXT ( 'NONE', 'WORKASPACE' ) );
#1685 = ORIENTED_EDGE ( 'NONE', *, *, #1425, .T. ) ;
#1686 = CARTESIAN_POINT ( 'NONE',  ( 609.8754609228352592, 185.7164421964179439, 185.4807968138250374 ) ) ;
#1687 = ADVANCED_FACE ( 'NONE', ( #6948 ), #5621, .T. ) ;
#1688 = B_SPLINE_CURVE_WITH_KNOTS ( 'NONE', 3,
 ( #6289, #13426, #3240, #12232, #2123, #4097 ),
 .UNSPECIFIED., .F., .F.,
 ( 4, 2, 4 ),
 ( 0.01237452868098001986, 0.01354396209252427784, 0.01471339550406853582 ),
 .UNSPECIFIED. ) ;
#1689 = CARTESIAN_POINT ( 'NONE',  ( 610.3687250539534261, 189.1718658564638247, -186.1427899493634470 ) ) ;
#1690 = CARTESIAN_POINT ( 'NONE',  ( 440.1783540539412343, 278.3868002927283101, 210.0000000000000000 ) ) ;
#1691 = CIRCLE ( 'NONE', #14422, 2.041999999999999815 ) ;
#1692 = CARTESIAN_POINT ( 'NONE',  ( -0.1410422978106123659, 4.700232962125094893, -3.687027686973624707 ) ) ;
#1693 = ORIENTED_EDGE ( 'NONE', *, *, #9766, .T. ) ;
#1694 = LINE ( 'NONE', #5094, #156 ) ;
#1695 = EDGE_LOOP ( 'NONE', ( #14289, #6398, #3405, #4458 ) ) ;
#1696 = ADVANCED_FACE ( 'NONE', ( #6187 ), #9866, .T. ) ;
#1697 = EDGE_CURVE ( 'NONE', #9831, #3784, #6454, .T. ) ;
#1698 = ORIENTED_EDGE ( 'NONE', *, *, #12361, .T. ) ;
#1699 =( NAMED_UNIT ( * ) PLANE_ANGLE_UNIT ( ) SI_UNIT ( $, .RADIAN. ) );
#1700 = ADVANCED_FACE ( 'NONE', ( #4672 ), #3415, .T. ) ;
#1701 = CARTESIAN_POINT ( 'NONE',  ( 3.811597179862312057, -5.304926841629219680, -0.01956314070068839589 ) ) ;
#1702 = AXIS2_PLACEMENT_3D ( 'NONE', #4505, #4645, #1165 ) ;
#1703 = CARTESIAN_POINT ( 'NONE',  ( 112.9652219749295341, 376.5507399164317803, 210.0000000000000000 ) ) ;
#1704 = PRODUCT_DEFINITION_SHAPE ( 'NONE', 'NONE',  #14626 ) ;
#1705 = CARTESIAN_POINT ( 'NONE',  ( 640.0000000000000000, 160.0000000000000284, -222.5000000000000000 ) ) ;
#1706 = AXIS2_PLACEMENT_3D ( 'NONE', #2511, #11446, #7017 ) ;
#1707 = CARTESIAN_POINT ( 'NONE',  ( 148.9991633467111569, 386.6211705227183870, 210.0000000000000000 ) ) ;
#1708 = VERTEX_POINT ( 'NONE', #10205 ) ;
#1709 = CARTESIAN_POINT ( 'NONE',  ( 0.000000000000000000, 0.5192545390863916310, -1.000000000000000000 ) ) ;
#1710 = FACE_OUTER_BOUND ( 'NONE', #14218, .T. ) ;
#1711 =( LENGTH_UNIT ( ) NAMED_UNIT ( * ) SI_UNIT ( .MILLI., .METRE. ) );
#1712 = CIRCLE ( 'NONE', #2179, 5.525000000000000355 ) ;
#1713 = ADVANCED_FACE ( 'NONE', ( #209 ), #4604, .T. ) ;
#1714 = DIRECTION ( 'NONE',  ( -0.2873478855663453291, -0.9578262852211513190, -3.835990623682899812E-15 ) ) ;
#1715 = EDGE_LOOP ( 'NONE', ( #3495, #11886, #10893, #12501, #10491 ) ) ;
#1716 = VERTEX_POINT ( 'NONE', #12628 ) ;
#1717 = FACE_OUTER_BOUND ( 'NONE', #6938, .T. ) ;
#1718 = PLANE ( 'NONE',  #13443 ) ;
#1719 = CARTESIAN_POINT ( 'NONE',  ( 609.9288325809317257, 190.4177448864037956, -189.9663414180174925 ) ) ;
#1720 = CIRCLE ( 'NONE', #13740, 5.000000000000004441 ) ;
#1721 = CYLINDRICAL_SURFACE ( 'NONE', #1389, 5.000000000000004441 ) ;
#1722 = ORIENTED_EDGE ( 'NONE', *, *, #3760, .F. ) ;
#1723 = ADVANCED_FACE ( 'NONE', ( #12779 ), #9600, .T. ) ;
#1724 = PLANE ( 'NONE',  #5734 ) ;
#1725 = DIRECTION ( 'NONE',  ( -0.2873478855663455511, -0.9578262852211514300, 4.074758502541097232E-16 ) ) ;
#1726 = EDGE_CURVE ( 'NONE', #9048, #852, #1552, .T. ) ;
#1727 = DIRECTION ( 'NONE',  ( 0.000000000000000000, 0.000000000000000000, -1.000000000000000000 ) ) ;
#1728 = DIRECTION ( 'NONE',  ( 9.794481010665704304E-16, 3.264827003555234768E-15, -1.000000000000000000 ) ) ;
#1729 = VERTEX_POINT ( 'NONE', #1770 ) ;
#1730 = CARTESIAN_POINT ( 'NONE',  ( 3.809068165403724393, 5.306386968807659699, 9.757819552369535962E-16 ) ) ;
#1731 = ORIENTED_EDGE ( 'NONE', *, *, #11221, .F. ) ;
#1732 = ORIENTED_EDGE ( 'NONE', *, *, #498, .F. ) ;
#1733 = DIRECTION ( 'NONE',  ( 0.000000000000000000, 0.000000000000000000, 1.000000000000000000 ) ) ;
#1734 = CIRCLE ( 'NONE', #12322, 2.649999999999985700 ) ;
#1735 = CARTESIAN_POINT ( 'NONE',  ( 0.000000000000000000, 0.000000000000000000, 3.469446951953614189E-15 ) ) ;
#1736 = CARTESIAN_POINT ( 'NONE',  ( 0.4465819873851995525, 2.886751345948122882, -5.000000000000000000 ) ) ;
#1737 = FACE_OUTER_BOUND ( 'NONE', #12077, .T. ) ;
#1738 = ORIENTED_EDGE ( 'NONE', *, *, #7077, .F. ) ;
#1739 = CARTESIAN_POINT ( 'NONE',  ( -1.500000000000001332, 0.000000000000000000, 0.000000000000000000 ) ) ;
#1740 = DIRECTION ( 'NONE',  ( 0.000000000000000000, 0.000000000000000000, -1.000000000000000000 ) ) ;
#1741 = CARTESIAN_POINT ( 'NONE',  ( 148.9991633467111569, 386.6211705227183870, -210.0000000000000000 ) ) ;
#1742 = SURFACE_STYLE_FILL_AREA ( #2639 ) ;
#1743 = ORIENTED_EDGE ( 'NONE', *, *, #13399, .T. ) ;
#1744 = CARTESIAN_POINT ( 'NONE',  ( 706.6446721788141758, 159.8177707722969956, 177.6000000000005627 ) ) ;
#1745 = CARTESIAN_POINT ( 'NONE',  ( 139.8040310085880833, 355.9707293956415697, 187.0000000000000000 ) ) ;
#1746 = ORIENTED_EDGE ( 'NONE', *, *, #3611, .F. ) ;
#1747 = CARTESIAN_POINT ( 'NONE',  ( 6.367873360227556567, 2.886751345948125547, 4.999999999999999112 ) ) ;
#1748 = EDGE_CURVE ( 'NONE', #6946, #6153, #12852, .T. ) ;
#1749 = CARTESIAN_POINT ( 'NONE',  ( 0.000000000000000000, 3.464101615137751278, -2.000000000000006217 ) ) ;
#1750 = CARTESIAN_POINT ( 'NONE',  ( 627.5000000000000000, 160.0000000000000284, 207.0000000000000000 ) ) ;
#1751 = ORIENTED_EDGE ( 'NONE', *, *, #5498, .F. ) ;
#1752 = DIRECTION ( 'NONE',  ( 1.000000000000000000, 9.498873539028489960E-17, 0.000000000000000000 ) ) ;
#1753 = DIRECTION ( 'NONE',  ( -1.000000000000000000, -0.000000000000000000, -0.000000000000000000 ) ) ;
#1754 = CARTESIAN_POINT ( 'NONE',  ( 4.000000000000000000, 2.309401076758515803, -0.4999999999999995559 ) ) ;
#1755 = FACE_OUTER_BOUND ( 'NONE', #3068, .T. ) ;
#1756 = ORIENTED_EDGE ( 'NONE', *, *, #1901, .F. ) ;
#1757 = ORIENTED_EDGE ( 'NONE', *, *, #9309, .F. ) ;
#1758 = VERTEX_POINT ( 'NONE', #14040 ) ;
#1759 = CARTESIAN_POINT ( 'NONE',  ( 6.500000000000005329, -3.752776749732571027, -6.177805531629060987 ) ) ;
#1760 = EDGE_CURVE ( 'NONE', #14191, #12163, #1134, .T. ) ;
#1761 = CARTESIAN_POINT ( 'NONE',  ( -1.500000000000001332, 0.000000000000000000, 0.000000000000000000 ) ) ;
#1762 = ADVANCED_FACE ( 'NONE', ( #581 ), #13002, .F. ) ;
#1763 = CARTESIAN_POINT ( 'NONE',  ( 642.5000994061915662, 160.9940618269907020, -209.9999999999999716 ) ) ;
#1764 = DIRECTION ( 'NONE',  ( -0.000000000000000000, -0.000000000000000000, 1.000000000000000000 ) ) ;
#1765 = EDGE_CURVE ( 'NONE', #11111, #7982, #8342, .T. ) ;
#1766 = UNCERTAINTY_MEASURE_WITH_UNIT (LENGTH_MEASURE( 1.000000000000000082E-05 ), #1303, 'distance_accuracy_value', 'NONE');
#1767 = DIRECTION ( 'NONE',  ( -1.000000000000000000, 0.000000000000000000, 0.000000000000000000 ) ) ;
#1768 = EDGE_LOOP ( 'NONE', ( #1792, #14548 ) ) ;
#1769 = EDGE_CURVE ( 'NONE', #12254, #9582, #9397, .T. ) ;
#1770 = CARTESIAN_POINT ( 'NONE',  ( 451.6722694765949768, 316.6998517015743460, 190.0000000000000000 ) ) ;
#1771 = CARTESIAN_POINT ( 'NONE',  ( 3.700000000000000178, 0.000000000000000000, 0.000000000000000000 ) ) ;
#1772 = SHAPE_DEFINITION_REPRESENTATION ( #11462, #1780 ) ;
#1773 = DIRECTION ( 'NONE',  ( -0.9237280213470676626, -0.3830490080632388272, 0.000000000000000000 ) ) ;
#1774 = ORIENTED_EDGE ( 'NONE', *, *, #9647, .T. ) ;
#1775 = EDGE_LOOP ( 'NONE', ( #12688, #11502, #5375, #9233 ) ) ;
#1776 = CYLINDRICAL_SURFACE ( 'NONE', #10557, 4.199999999999981526 ) ;
#1777 = CARTESIAN_POINT ( 'NONE',  ( -10.00000000000007105, 413.4403065089107372, 184.7999999999999829 ) ) ;
#1778 = CARTESIAN_POINT ( 'NONE',  ( -5.560781378645573980, 0.000000000000000000, -4.000000000000000000 ) ) ;
#1779 = APPLICATION_CONTEXT ( 'automotive_design' ) ;
#1780 = SHAPE_REPRESENTATION ( 'hex flange nut gradea_iso_ISO - 4161 - M8 - N', ( #9440 ), #13250 ) ;
#1781 = DIRECTION ( 'NONE',  ( 1.000000000000000000, 0.000000000000000000, 0.000000000000000000 ) ) ;
#1782 = ADVANCED_FACE ( 'NONE', ( #519 ), #7170, .T. ) ;
#1783 = ORIENTED_EDGE ( 'NONE', *, *, #10703, .F. ) ;
#1784 = EDGE_CURVE ( 'NONE', #3368, #1845, #5988, .T. ) ;
#1785 = DIRECTION ( 'NONE',  ( 0.000000000000000000, 0.000000000000000000, -1.000000000000000000 ) ) ;
#1786 = CYLINDRICAL_SURFACE ( 'NONE', #6427, 4.000000000000000000 ) ;
#1787 = FACE_OUTER_BOUND ( 'NONE', #14245, .T. ) ;
#1788 = ADVANCED_FACE ( 'NONE', ( #2810 ), #13888, .T. ) ;
#1789 = LINE ( 'NONE', #2689, #13155 ) ;
#1790 = CARTESIAN_POINT ( 'NONE',  ( 43.50000000000000711, 0.000000000000000000, 3.309499999999999886 ) ) ;
#1791 = CARTESIAN_POINT ( 'NONE',  ( -10.00000000000000000, 371.6790804732683569, 187.0000000000000000 ) ) ;
#1792 = ORIENTED_EDGE ( 'NONE', *, *, #10146, .T. ) ;
#1793 = CARTESIAN_POINT ( 'NONE',  ( 8.500000000000000000, 5.773502691896261751, 0.000000000000000000 ) ) ;
#1794 = VERTEX_POINT ( 'NONE', #437 ) ;
#1795 = EDGE_LOOP ( 'NONE', ( #11184, #269, #706, #1589, #3816, #4469 ) ) ;
#1796 = CARTESIAN_POINT ( 'NONE',  ( 610.8620436566991430, 230.3137853645733912, -184.7999999999999829 ) ) ;
#1797 = DIRECTION ( 'NONE',  ( 0.000000000000000000, 0.000000000000000000, -1.000000000000000000 ) ) ;
#1798 = CARTESIAN_POINT ( 'NONE',  ( 635.0000000000000000, 160.0000000000000284, -207.0000000000000000 ) ) ;
#1799 = CARTESIAN_POINT ( 'NONE',  ( 631.0000000000000000, 155.9999999999999432, -233.5000000000000000 ) ) ;
#1800 = ORIENTED_EDGE ( 'NONE', *, *, #6923, .F. ) ;
#1801 = CARTESIAN_POINT ( 'NONE',  ( 6.390983399715590707, -2.822795037344613789, 5.110775575965826434 ) ) ;
#1802 = LINE ( 'NONE', #11845, #13199 ) ;
#1803 = CARTESIAN_POINT ( 'NONE',  ( 0.1920286436967153787, 7.516269729766880368E-16, -5.525000000000000355 ) ) ;
#1804 = DIRECTION ( 'NONE',  ( -1.000000000000000000, 0.000000000000000000, 0.000000000000000000 ) ) ;
#1805 = PRESENTATION_STYLE_ASSIGNMENT (( #2092 ) ) ;
#1806 = EDGE_LOOP ( 'NONE', ( #10812, #11402, #13673 ) ) ;
#1807 =( NAMED_UNIT ( * ) SI_UNIT ( $, .STERADIAN. ) SOLID_ANGLE_UNIT ( ) );
#1808 = CARTESIAN_POINT ( 'NONE',  ( 443.6584422793565636, 264.0194060144110608, 187.0000000000000000 ) ) ;
#1809 = CONTEXT_DEPENDENT_SHAPE_REPRESENTATION ( #4437, #13370 ) ;
#1810 = ORIENTED_EDGE ( 'NONE', *, *, #2803, .F. ) ;
#1811 = VECTOR ( 'NONE', #8380, 1000.000000000000227 ) ;
#1812 = DIRECTION ( 'NONE',  ( 1.000000000000000000, 0.000000000000000000, 0.000000000000000000 ) ) ;
#1813 = DIRECTION ( 'NONE',  ( 0.000000000000000000, 1.000000000000000000, 0.000000000000000000 ) ) ;
#1814 = B_SPLINE_CURVE_WITH_KNOTS ( 'NONE', 3,
 ( #5921, #14043, #11728, #6143, #10425, #12705, #13816, #12784, #356, #13892, #2676, #3712, #8193, #2600, #3927, #7098 ),
 .UNSPECIFIED., .F., .F.,
 ( 4, 3, 3, 3, 3, 4 ),
 ( 0.000000000000000000, 5.303647860849296453E-05, 0.0001057093501027513691, 0.0001642058037233857007, 0.0002210073443967692478, 0.0002236769549551747692 ),
 .UNSPECIFIED. ) ;
#1815 = ORIENTED_EDGE ( 'NONE', *, *, #12410, .T. ) ;
#1816 = DIRECTION ( 'NONE',  ( 0.000000000000000000, 0.000000000000000000, 1.000000000000000000 ) ) ;
#1817 = CARTESIAN_POINT ( 'NONE',  ( -3.999999999999999112, 0.000000000000000000, -7.974599999999998801 ) ) ;
#1818 = AXIS2_PLACEMENT_3D ( 'NONE', #1741, #480, #11630 ) ;
#1819 = CARTESIAN_POINT ( 'NONE',  ( 610.5828669213532294, 188.7537838752662935, -185.5093481647506906 ) ) ;
#1820 =( LENGTH_UNIT ( ) NAMED_UNIT ( * ) SI_UNIT ( .MILLI., .METRE. ) );
#1821 = EDGE_CURVE ( 'NONE', #12673, #7913, #13600, .T. ) ;
#1822 = ORIENTED_EDGE ( 'NONE', *, *, #9164, .T. ) ;
#1824 = EDGE_CURVE ( 'NONE', #9269, #7982, #8456, .T. ) ;
#1823 = SURFACE_STYLE_FILL_AREA ( #2719 ) ;
#1825 = CARTESIAN_POINT ( 'NONE',  ( -6.500000000000000888, 0.6470732608156811727, -0.01945970098673090176 ) ) ;
#1826 = EDGE_LOOP ( 'NONE', ( #9063, #13172, #6884, #1878 ) ) ;
#1827 = ORIENTED_EDGE ( 'NONE', *, *, #4130, .F. ) ;
#1828 = CARTESIAN_POINT ( 'NONE',  ( 610.8620436566991430, 188.5525593289318351, -169.9999999999999716 ) ) ;
#1829 = AXIS2_PLACEMENT_3D ( 'NONE', #13037, #2924, #7421 ) ;
#1831 = VECTOR ( 'NONE', #3586, 1000.000000000000000 ) ;
#1830 = FACE_BOUND ( 'NONE', #8586, .T. ) ;
#1832 = LINE ( 'NONE', #2888, #9216 ) ;
#1833 = DIRECTION ( 'NONE',  ( 1.000000000000000000, 0.000000000000000000, 0.000000000000000000 ) ) ;
#1834 = CARTESIAN_POINT ( 'NONE',  ( -6.815830331203685866, -1.210827632163352847E-13, -6.171384342982610960 ) ) ;
#1835 = EDGE_CURVE ( 'NONE', #8255, #6536, #14349, .T. ) ;
#1836 = VERTEX_POINT ( 'NONE', #9467 ) ;
#1837 = ADVANCED_FACE ( 'NONE', ( #2596 ), #7235, .T. ) ;
#1838 = CIRCLE ( 'NONE', #896, 6.080745460913608902 ) ;
#1839 = CIRCLE ( 'NONE', #5617, 2.649999999999985700 ) ;
#1840 = AXIS2_PLACEMENT_3D ( 'NONE', #14104, #9680, #1490 ) ;
#1841 = DIRECTION ( 'NONE',  ( 0.000000000000000000, 0.000000000000000000, 1.000000000000000000 ) ) ;
#1842 = LINE ( 'NONE', #9892, #907 ) ;
#1843 = APPLICATION_PROTOCOL_DEFINITION ( 'draft international standard', 'automotive_design', 1998, #3018 ) ;
#1844 = CARTESIAN_POINT ( 'NONE',  ( 604.3113219698374223, -181.2933965909537903, 177.6000000000015575 ) ) ;
#1845 = VERTEX_POINT ( 'NONE', #6213 ) ;
#1846 = ORIENTED_EDGE ( 'NONE', *, *, #5206, .F. ) ;
#1847 = CARTESIAN_POINT ( 'NONE',  ( 611.4942090049448780, 232.4210031920598283, 187.0000000000000000 ) ) ;
#1848 = CARTESIAN_POINT ( 'NONE',  ( 4.000000000000000000, 0.000000000000000000, -8.000000000000000000 ) ) ;
#1849 = ADVANCED_FACE ( 'NONE', ( #10641 ), #653, .F. ) ;
#1850 = CARTESIAN_POINT ( 'NONE',  ( -3.755786496842903988E-16, -7.505553499465146494, -6.064240316920404439 ) ) ;
#1851 = CIRCLE ( 'NONE', #7037, 5.199999999999760369 ) ;
#1852 = CIRCLE ( 'NONE', #2573, 5.000000000000000000 ) ;
#1853 = DIRECTION ( 'NONE',  ( 0.000000000000000000, 0.000000000000000000, 1.000000000000000000 ) ) ;
#1854 = ORIENTED_EDGE ( 'NONE', *, *, #10722, .F. ) ;
#1855 = CARTESIAN_POINT ( 'NONE',  ( 610.0000000000000000, 0.000000000000000000, 190.0000000000000000 ) ) ;
#1856 = CARTESIAN_POINT ( 'NONE',  ( 4.000000000000000888, 1.563622288139206118, -0.2253451193528334950 ) ) ;
#1857 = DIRECTION ( 'NONE',  ( -1.000000000000000000, 0.000000000000000000, 0.000000000000000000 ) ) ;
#1858 = EDGE_CURVE ( 'NONE', #5524, #13510, #8711, .T. ) ;
#1859 = VERTEX_POINT ( 'NONE', #1923 ) ;
#1860 = AXIS2_PLACEMENT_3D ( 'NONE', #10254, #5816, #9141 ) ;
#1861 = FACE_OUTER_BOUND ( 'NONE', #4687, .T. ) ;
#1862 = CARTESIAN_POINT ( 'NONE',  ( 721.0120664571321640, 218.1493915422654766, 177.5999999999999659 ) ) ;
#1863 = DIRECTION ( 'NONE',  ( 0.1305261922200524616, 0.9914448613738103822, -0.000000000000000000 ) ) ;
#1864 = SHAPE_REPRESENTATION_RELATIONSHIP ( 'NONE' , 'NONE' ,  #5462, #13030 ) ;
#1865 = ORIENTED_EDGE ( 'NONE', *, *, #6557, .T. ) ;
#1866 = VECTOR ( 'NONE', #645, 1000.000000000000227 ) ;
#1867 = CIRCLE ( 'NONE', #6348, 5.000000000000004441 ) ;
#1868 = ORIENTED_EDGE ( 'NONE', *, *, #11880, .F. ) ;
#1869 = EDGE_LOOP ( 'NONE', ( #5841, #9339, #9809, #5523 ) ) ;
#1870 = ADVANCED_FACE ( 'NONE', ( #13141 ), #5390, .T. ) ;
#1871 = CARTESIAN_POINT ( 'NONE',  ( 590.0000000000000000, 212.5596934910894333, -190.0000000000000000 ) ) ;
#1872 = ADVANCED_FACE ( 'NONE', ( #4292 ), #6434, .T. ) ;
#1873 = SHAPE_REPRESENTATION ( 'main frame', ( #9440 ), #7553 ) ;
#1874 = ADVANCED_FACE ( 'NONE', ( #6352 ), #6796, .T. ) ;
#1875 = CARTESIAN_POINT ( 'NONE',  ( 0.000000000000000000, 0.000000000000000000, 4.000000000000000000 ) ) ;
#1876 = PRODUCT_RELATED_PRODUCT_CATEGORY ( 'part', '', ( #9107 ) ) ;
#1877 = AXIS2_PLACEMENT_3D ( 'NONE', #12827, #1682, #13942 ) ;
#1878 = ORIENTED_EDGE ( 'NONE', *, *, #11509, .T. ) ;
#1879 = AXIS2_PLACEMENT_3D ( 'NONE', #1351, #12641, #147 ) ;
#1880 = VERTEX_POINT ( 'NONE', #10931 ) ;
#1881 = CARTESIAN_POINT ( 'NONE',  ( 635.0000000000000000, 160.0000000000000284, 187.5000000000000000 ) ) ;
#1882 = CARTESIAN_POINT ( 'NONE',  ( 6.500000000000000888, 1.355443906731431669, -5.756734754743127347 ) ) ;
#1883 = PLANE ( 'NONE',  #4671 ) ;
#1884 = DIRECTION ( 'NONE',  ( 0.000000000000000000, 0.000000000000000000, -1.000000000000000000 ) ) ;
#1885 = AXIS2_PLACEMENT_3D ( 'NONE', #11601, #12788, #8198 ) ;
#1886 = ORIENTED_EDGE ( 'NONE', *, *, #5597, .F. ) ;
#1887 = VECTOR ( 'NONE', #8738, 1000.000000000000000 ) ;
#1888 = CARTESIAN_POINT ( 'NONE',  ( 609.7983275391768530, 185.9141716657875349, 186.1519484124941641 ) ) ;
#1889 = FACE_OUTER_BOUND ( 'NONE', #13103, .T. ) ;
#1890 = EDGE_LOOP ( 'NONE', ( #7121, #1010, #6690, #9370 ) ) ;
#1891 = DIRECTION ( 'NONE',  ( -0.9578262852211513190, 0.2873478855663453846, 0.000000000000000000 ) ) ;
#1892 = ORIENTED_EDGE ( 'NONE', *, *, #3203, .F. ) ;
#1893 = LINE ( 'NONE', #2781, #8946 ) ;
#1894 = CONICAL_SURFACE ( 'NONE', #2838, 2.500000000000000888, 0.9599310885968785900 ) ;
#1895 = VECTOR ( 'NONE', #8715, 1000.000000000000114 ) ;
#1896 = CARTESIAN_POINT ( 'NONE',  ( 629.7500000000000000, 160.0000000000000284, -210.0000000000000000 ) ) ;
#1897 = VERTEX_POINT ( 'NONE', #14472 ) ;
#1898 = DIRECTION ( 'NONE',  ( 0.9578262852211513190, -0.2873478855663453846, -0.000000000000000000 ) ) ;
#1899 = DIRECTION ( 'NONE',  ( 1.000000000000000000, 0.000000000000000000, 0.000000000000000000 ) ) ;
#1900 = CIRCLE ( 'NONE', #10153, 7.000000000000000000 ) ;
#1901 = EDGE_CURVE ( 'NONE', #4077, #8268, #9755, .T. ) ;
#1902 = PRESENTATION_LAYER_ASSIGNMENT (  '', '', ( #1675 ) ) ;
#1903 = DIRECTION ( 'NONE',  ( 0.000000000000000000, 0.000000000000000000, 1.000000000000000000 ) ) ;
#1904 = PRESENTATION_STYLE_ASSIGNMENT (( #3013 ) ) ;
#1905 = EDGE_LOOP ( 'NONE', ( #2174, #8731, #3580, #11453 ) ) ;
#1906 = EDGE_CURVE ( 'NONE', #8019, #4246, #12164, .T. ) ;
#1907 = CARTESIAN_POINT ( 'NONE',  ( 6.355827204229362870, 3.436818823786758070, 4.264647808192652434 ) ) ;
#1908 = CARTESIAN_POINT ( 'NONE',  ( -6.500000000000000000, 2.536640449112271156, -0.3753468889000206032 ) ) ;
#1909 = ORIENTED_EDGE ( 'NONE', *, *, #2407, .F. ) ;
#1910 = AXIS2_PLACEMENT_3D ( 'NONE', #350, #8568, #2730 ) ;
#1911 = VECTOR ( 'NONE', #7042, 1000.000000000000227 ) ;
#1912 = VERTEX_POINT ( 'NONE', #14396 ) ;
#1913 = VECTOR ( 'NONE', #90, 1000.000000000000000 ) ;
#1914 = PRESENTATION_LAYER_ASSIGNMENT (  '', '', ( #6154 ) ) ;
#1915 = DIRECTION ( 'NONE',  ( -0.000000000000000000, -0.000000000000000000, 1.000000000000000000 ) ) ;
#1916 = DIRECTION ( 'NONE',  ( -0.000000000000000000, -0.000000000000000000, -1.000000000000000000 ) ) ;
#1917 = EDGE_CURVE ( 'NONE', #5125, #8805, #1025, .T. ) ;
#1918 = AXIS2_PLACEMENT_3D ( 'NONE', #7664, #12083, #13271 ) ;
#1919 = CARTESIAN_POINT ( 'NONE',  ( 636.7009106935324780, 155.5114698605638637, -210.0000000000000000 ) ) ;
#1920 = AXIS2_PLACEMENT_3D ( 'NONE', #3888, #7564, #11017 ) ;
#1921 = CARTESIAN_POINT ( 'NONE',  ( 639.0000000000000000, 164.0000000000000000, -233.5000000000000000 ) ) ;
#1922 = ORIENTED_EDGE ( 'NONE', *, *, #4212, .F. ) ;
#1923 = CARTESIAN_POINT ( 'NONE',  ( 716.7018481736365629, 193.3416907550376322, 182.8000000000001535 ) ) ;
#1924 = LINE ( 'NONE', #14397, #14128 ) ;
#1925 = CARTESIAN_POINT ( 'NONE',  ( 139.8040310085880833, 355.9707293956415697, -183.5000000000000000 ) ) ;
#1926 = CARTESIAN_POINT ( 'NONE',  ( 610.0000000000001137, 185.6790804732684421, -184.8000000000000682 ) ) ;
#1927 = ORIENTED_EDGE ( 'NONE', *, *, #5206, .T. ) ;
#1928 = ORIENTED_EDGE ( 'NONE', *, *, #5544, .T. ) ;
#1929 = AXIS2_PLACEMENT_3D ( 'NONE', #1881, #9719, #771 ) ;
#1930 = DIRECTION ( 'NONE',  ( 0.000000000000000000, 0.000000000000000000, -1.000000000000000000 ) ) ;
#1931 = DIRECTION ( 'NONE',  ( -0.000000000000000000, -0.000000000000000000, 1.000000000000000000 ) ) ;
#1932 = LINE ( 'NONE', #6222, #12954 ) ;
#1933 = ADVANCED_FACE ( 'NONE', ( #6571 ), #14256, .F. ) ;
#1934 = COLOUR_RGB ( '',1.000000000000000000, 0.9490196078431372140, 0.9098039215686274384 ) ;
#1935 = CARTESIAN_POINT ( 'NONE',  ( 0.5619217318086654478, 7.564468822943301696, -6.443866470201762731 ) ) ;
#1936 = VERTEX_POINT ( 'NONE', #10990 ) ;
#1937 = UNCERTAINTY_MEASURE_WITH_UNIT (LENGTH_MEASURE( 1.000000000000000082E-05 ), #10196, 'distance_accuracy_value', 'NONE');
#1938 = AXIS2_PLACEMENT_3D ( 'NONE', #9662, #6257, #4942 ) ;
#1939 = CARTESIAN_POINT ( 'NONE',  ( -6.826580258811596025, 2.695816818222440681, -6.331007506863580048 ) ) ;
#1940 = ORIENTED_EDGE ( 'NONE', *, *, #5847, .F. ) ;
#1941 = CIRCLE ( 'NONE', #11374, 7.900000000000002132 ) ;
#1942 = CARTESIAN_POINT ( 'NONE',  ( 650.0000000000000000, 145.0000000000000568, -210.0000000000000000 ) ) ;
#1943 = CARTESIAN_POINT ( 'NONE',  ( 2.999999999999999112, 2.309401076758500704, -4.000000000000000000 ) ) ;
#1944 = DIRECTION ( 'NONE',  ( 0.000000000000000000, 0.000000000000000000, -1.000000000000000000 ) ) ;
#1945 = ORIENTED_EDGE ( 'NONE', *, *, #14180, .T. ) ;
#1946 = AXIS2_PLACEMENT_3D ( 'NONE', #13668, #4825, #12703 ) ;
#1947 = CARTESIAN_POINT ( 'NONE',  ( -4.000000000000000000, -2.309401076758512694, -3.433295621305382461 ) ) ;
#1948 = ORIENTED_EDGE ( 'NONE', *, *, #1428, .T. ) ;
#1949 = VERTEX_POINT ( 'NONE', #4078 ) ;
#1950 = CARTESIAN_POINT ( 'NONE',  ( 0.000000000000000000, 0.000000000000000000, 0.000000000000000000 ) ) ;
#1951 = VECTOR ( 'NONE', #3608, 1000.000000000000227 ) ;
#1952 = EDGE_CURVE ( 'NONE', #12984, #14237, #14267, .T. ) ;
#1953 = DIRECTION ( 'NONE',  ( 1.000000000000000000, 0.000000000000000000, 0.000000000000000000 ) ) ;
#1954 = EDGE_CURVE ( 'NONE', #10044, #10356, #14320, .T. ) ;
#1955 = EDGE_LOOP ( 'NONE', ( #9013, #4556, #6062, #1255 ) ) ;
#1956 = ORIENTED_EDGE ( 'NONE', *, *, #5983, .T. ) ;
#1957 = CARTESIAN_POINT ( 'NONE',  ( 702.5260191523640287, 164.1854586329053518, -177.6000000000005059 ) ) ;
#1958 = CARTESIAN_POINT ( 'NONE',  ( 629.0024986820136519, 164.6091003998119220, 210.0000119999999981 ) ) ;
#1959 = ADVANCED_FACE ( 'NONE', ( #8571 ), #1578, .T. ) ;
#1960 = CARTESIAN_POINT ( 'NONE',  ( -0.5449313310646672903, -4.304185902836978883, -3.316620875263469159 ) ) ;
#1961 = LINE ( 'NONE', #10363, #9746 ) ;
#1962 =( NAMED_UNIT ( * ) PLANE_ANGLE_UNIT ( ) SI_UNIT ( $, .RADIAN. ) );
#1963 = MECHANICAL_DESIGN_GEOMETRIC_PRESENTATION_REPRESENTATION (  '', ( #51 ), #14000 ) ;
#1964 = ORIENTED_EDGE ( 'NONE', *, *, #8270, .T. ) ;
#1966 = EDGE_CURVE ( 'NONE', #7989, #9048, #9818, .T. ) ;
#1965 = CIRCLE ( 'NONE', #3861, 0.1000000000000002554 ) ;
#1967 = DIRECTION ( 'NONE',  ( 0.9578262852211489875, -0.2873478855663534892, 0.000000000000000000 ) ) ;
#1968 = ORIENTED_EDGE ( 'NONE', *, *, #9334, .T. ) ;
#1969 = CARTESIAN_POINT ( 'NONE',  ( -4.799999999999999822, 5.878304635907294211E-16, 0.000000000000000000 ) ) ;
#1970 = ORIENTED_EDGE ( 'NONE', *, *, #5113, .F. ) ;
#1971 = LINE ( 'NONE', #5302, #12719 ) ;
#1972 = CARTESIAN_POINT ( 'NONE',  ( 0.1973348417602471538, -1.936114729415142399, 4.999999999999999112 ) ) ;
#1973 = EDGE_LOOP ( 'NONE', ( #5043, #10935, #6632, #46 ) ) ;
#1974 = DIRECTION ( 'NONE',  ( -1.000000000000000000, 0.000000000000000000, 0.000000000000000000 ) ) ;
#1975 = EDGE_CURVE ( 'NONE', #1729, #6382, #7613, .T. ) ;
#1976 = EDGE_CURVE ( 'NONE', #783, #5188, #12100, .T. ) ;
#1977 = CARTESIAN_POINT ( 'NONE',  ( 2.500000000000000000, -1.178949249685214307, 2.042000000000001592 ) ) ;
#1978 = ORIENTED_EDGE ( 'NONE', *, *, #8265, .F. ) ;
#1979 = EDGE_CURVE ( 'NONE', #5923, #7944, #14323, .T. ) ;
#1980 = DIRECTION ( 'NONE',  ( -1.000000000000000000, -0.000000000000000000, -0.000000000000000000 ) ) ;
#1981 = CARTESIAN_POINT ( 'NONE',  ( 611.4942090049451053, 232.4210031920599135, -187.0000000000000000 ) ) ;
#1982 = ORIENTED_EDGE ( 'NONE', *, *, #13598, .F. ) ;
#1983 = APPLICATION_CONTEXT ( 'automotive_design' ) ;
#1984 = EDGE_LOOP ( 'NONE', ( #1143, #10346, #3079 ) ) ;
#1985 = CARTESIAN_POINT ( 'NONE',  ( 455.5035746174796714, 294.6698471414878782, -210.0000000000000000 ) ) ;
#1986 = DIRECTION ( 'NONE',  ( -1.000000000000000000, -0.000000000000000000, -0.000000000000000000 ) ) ;
#1987 = DIRECTION ( 'NONE',  ( -1.000000000000000000, 0.000000000000000000, 0.000000000000000000 ) ) ;
#1988 = DIRECTION ( 'NONE',  ( 0.000000000000000000, 0.000000000000000000, 1.000000000000000000 ) ) ;
#1989 = CARTESIAN_POINT ( 'NONE',  ( 2.999999999999999112, -3.464101615137757051, -1.999999999999996669 ) ) ;
#1990 = EDGE_LOOP ( 'NONE', ( #5741, #984, #8590, #6479, #10508, #8888, #12809, #6092 ) ) ;
#1991 = CARTESIAN_POINT ( 'NONE',  ( 642.5000000000001137, 160.0000000000000284, -210.0000119999999981 ) ) ;
#1992 = CARTESIAN_POINT ( 'NONE',  ( 6.270568613849416550, -4.911887854652846386, -1.704496029161937987 ) ) ;
#1993 = DIRECTION ( 'NONE',  ( -0.2873478855663453846, -0.9578262852211513190, -0.000000000000000000 ) ) ;
#1994 = ORIENTED_EDGE ( 'NONE', *, *, #8065, .T. ) ;
#1995 = VERTEX_POINT ( 'NONE', #6715 ) ;
#1996 = CARTESIAN_POINT ( 'NONE',  ( -10.00000000000000000, 413.4403065089105667, 190.0000000000000000 ) ) ;
#1997 = CARTESIAN_POINT ( 'NONE',  ( -6.500000000000000000, -3.752776749732572803, -6.064240316920399998 ) ) ;
#1998 = CARTESIAN_POINT ( 'NONE',  ( 6.500000000000001776, -5.204170427930421283E-15, -5.592027715088708995 ) ) ;
#1999 = ORIENTED_EDGE ( 'NONE', *, *, #2925, .T. ) ;
#2000 = DIRECTION ( 'NONE',  ( -1.000000000000000000, -0.000000000000000000, -0.000000000000000000 ) ) ;
#2001 = EDGE_LOOP ( 'NONE', ( #13223, #10824, #12086, #8874 ) ) ;
#2002 = CARTESIAN_POINT ( 'NONE',  ( 0.000000000000000000, 0.000000000000000000, -1.000000000000000000 ) ) ;
#2003 = DIRECTION ( 'NONE',  ( 0.000000000000000000, -1.000000000000000000, 0.000000000000000000 ) ) ;
#2004 = CARTESIAN_POINT ( 'NONE',  ( 628.0000000000000000, 235.0000000000000284, -225.5000000000000000 ) ) ;
#2005 = ADVANCED_FACE ( 'NONE', ( #7962 ), #6104, .F. ) ;
#2006 = EDGE_LOOP ( 'NONE', ( #3942, #13481, #136, #9943 ) ) ;
#2007 = CARTESIAN_POINT ( 'NONE',  ( 627.2408731339805854, 284.9098836221799615, -190.0000000000001990 ) ) ;
#2008 = VERTEX_POINT ( 'NONE', #4585 ) ;
#2009 = EDGE_LOOP ( 'NONE', ( #7216, #9637, #10310, #9166 ) ) ;
#2010 = CARTESIAN_POINT ( 'NONE',  ( 639.4338945024659324, 161.8386352387035743, -211.0000000000000000 ) ) ;
#2011 = FACE_OUTER_BOUND ( 'NONE', #10735, .T. ) ;
#2012 = CARTESIAN_POINT ( 'NONE',  ( -2.345747346278108214, 3.264484291692489215, -0.01223254789873409049 ) ) ;
#2013 = ORIENTED_EDGE ( 'NONE', *, *, #3123, .F. ) ;
#2014 = ORIENTED_EDGE ( 'NONE', *, *, #849, .T. ) ;
#2015 = CARTESIAN_POINT ( 'NONE',  ( 6.207671477327360243, -3.321994320370016407, 4.246137054663877919 ) ) ;
#2016 = DIRECTION ( 'NONE',  ( -1.000000000000000000, -0.000000000000000000, -0.000000000000000000 ) ) ;
#2017 = FACE_OUTER_BOUND ( 'NONE', #1333, .T. ) ;
#2018 = DIRECTION ( 'NONE',  ( -1.000000000000000000, 0.000000000000000000, 0.000000000000000000 ) ) ;
#2019 = CARTESIAN_POINT ( 'NONE',  ( 650.0000000000000000, 145.0000000000000568, 210.0000000000000000 ) ) ;
#2020 = SURFACE_SIDE_STYLE ('',( #2931 ) ) ;
#2021 = EDGE_CURVE ( 'NONE', #5281, #4527, #10031, .T. ) ;
#2022 = EDGE_LOOP ( 'NONE', ( #9325, #14476, #4318, #8173 ) ) ;
#2023 = CARTESIAN_POINT ( 'NONE',  ( 609.8615525982525014, 189.7413297629623514, 189.8335177487570888 ) ) ;
#2024 = EDGE_LOOP ( 'NONE', ( #6218, #423, #4699, #6724 ) ) ;
#2025 = CARTESIAN_POINT ( 'NONE',  ( 636.9746078850427011, 155.6249658629529620, 211.0000000000000000 ) ) ;
#2026 = ORIENTED_EDGE ( 'NONE', *, *, #3707, .F. ) ;
#2027 = EDGE_CURVE ( 'NONE', #4077, #13098, #3961, .T. ) ;
#2028 = EDGE_CURVE ( 'NONE', #10838, #1371, #12662, .T. ) ;
#2029 = DIRECTION ( 'NONE',  ( 0.9578262852211513190, -0.2873478855663453846, 1.110223024625157329E-15 ) ) ;
#2030 = CARTESIAN_POINT ( 'NONE',  ( 1.600000000000000089, 3.306546357697853733E-16, -2.700000000000000178 ) ) ;
#2031 = ORIENTED_EDGE ( 'NONE', *, *, #1457, .T. ) ;
#2032 = CARTESIAN_POINT ( 'NONE',  ( -10.00000000000000000, 10.00000000000000178, -210.0020000000000095 ) ) ;
#2033 = CARTESIAN_POINT ( 'NONE',  ( 631.0000000000000000, 164.0000000000000284, -225.5000000000000000 ) ) ;
#2034 = DIRECTION ( 'NONE',  ( 1.000000000000000000, 0.000000000000000000, -0.000000000000000000 ) ) ;
#2035 =( LENGTH_UNIT ( ) NAMED_UNIT ( * ) SI_UNIT ( .MILLI., .METRE. ) );
#2036 = ORIENTED_EDGE ( 'NONE', *, *, #6739, .T. ) ;
#2037 = B_SPLINE_CURVE_WITH_KNOTS ( 'NONE', 3,
 ( #3723, #8207, #12717, #2615, #10793, #14119 ),
 .UNSPECIFIED., .F., .F.,
 ( 4, 2, 4 ),
 ( 0.000000000000000000, 0.0002095117440864791795, 0.0004190234881729583589 ),
 .UNSPECIFIED. ) ;
#2038 = ORIENTED_EDGE ( 'NONE', *, *, #211, .T. ) ;
#2039 = ORIENTED_EDGE ( 'NONE', *, *, #6133, .F. ) ;
#2040 = CARTESIAN_POINT ( 'NONE',  ( 2.075968632162763061, -6.306992450856140131, -6.056431503344847478 ) ) ;
#2041 = ADVANCED_FACE ( 'NONE', ( #3327 ), #8042, .T. ) ;
#2042 = CARTESIAN_POINT ( 'NONE',  ( 631.2115189223973175, 153.4514063374357136, -210.0000000000000000 ) ) ;
#2043 = CARTESIAN_POINT ( 'NONE',  ( 6.500000000000000888, -2.534234941938116936, -0.3584823952106179212 ) ) ;
#2044 = AXIS2_PLACEMENT_3D ( 'NONE', #7770, #12258, #820 ) ;
#2045 = EDGE_CURVE ( 'NONE', #9831, #248, #3401, .T. ) ;
#2046 = VECTOR ( 'NONE', #12296, 1000.000000000000000 ) ;
#2047 = LINE ( 'NONE', #12096, #5443 ) ;
#2048 = CIRCLE ( 'NONE', #2765, 4.799999999999999822 ) ;
#2049 = CARTESIAN_POINT ( 'NONE',  ( 610.8620436566989156, 230.3137853645732775, 184.7999999999999829 ) ) ;
#2050 =( REPRESENTATION_RELATIONSHIP ('NONE','NONE', #2822, #3392 ) REPRESENTATION_RELATIONSHIP_WITH_TRANSFORMATION ( #9228 )SHAPE_REPRESENTATION_RELATIONSHIP( ) );
#2051 = ORIENTED_EDGE ( 'NONE', *, *, #3376, .T. ) ;
#2052 = CARTESIAN_POINT ( 'NONE',  ( 2.500000000000000000, 2.500728763858895382E-16, -2.041999999999999815 ) ) ;
#2053 = CYLINDRICAL_SURFACE ( 'NONE', #10817, 2.500000000000000444 ) ;
#2054 = AXIS2_PLACEMENT_3D ( 'NONE', #5135, #11687, #9343 ) ;
#2055 = DIRECTION ( 'NONE',  ( 0.000000000000000000, -1.000000000000000000, 0.000000000000000000 ) ) ;
#2056 = AXIS2_PLACEMENT_3D ( 'NONE', #3071, #2993, #6470 ) ;
#2057 = ORIENTED_EDGE ( 'NONE', *, *, #5293, .T. ) ;
#2058 = ORIENTED_EDGE ( 'NONE', *, *, #10606, .T. ) ;
#2059 = CARTESIAN_POINT ( 'NONE',  ( 2.999999999999999112, -4.618802153516999631, 0.000000000000000000 ) ) ;
#2060 = FACE_OUTER_BOUND ( 'NONE', #6298, .T. ) ;
#2061 = DIRECTION ( 'NONE',  ( 0.000000000000000000, -0.000000000000000000, -1.000000000000000000 ) ) ;
#2062 = CARTESIAN_POINT ( 'NONE',  ( -4.444974277457898637, 4.939246403833854160, -5.720331885005371930 ) ) ;
#2064 = ORIENTED_EDGE ( 'NONE', *, *, #13825, .F. ) ;
#2063 = COLOUR_RGB ( '',0.8941176470588234615, 0.8941176470588234615, 0.8941176470588234615 ) ;
#2065 = AXIS2_PLACEMENT_3D ( 'NONE', #9984, #3195, #2069 ) ;
#2066 = CARTESIAN_POINT ( 'NONE',  ( -6.500000000000000888, -2.727365451017189635, -5.874157743775032969 ) ) ;
#2067 = VERTEX_POINT ( 'NONE', #9142 ) ;
#2068 = ADVANCED_FACE ( 'NONE', ( #14211 ), #13648, .F. ) ;
#2069 = DIRECTION ( 'NONE',  ( 0.000000000000000000, -1.000000000000000000, 0.000000000000000000 ) ) ;
#2070 = LINE ( 'NONE', #9225, #10344 ) ;
#2071 = DIRECTION ( 'NONE',  ( 1.000000000000000000, 0.000000000000000000, 0.000000000000000000 ) ) ;
#2072 = EDGE_CURVE ( 'NONE', #2217, #12155, #10305, .T. ) ;
#2073 = CARTESIAN_POINT ( 'NONE',  ( -2.222614453595284090E-15, -0.3908539631446481533, 3.999999999999996447 ) ) ;
#2074 = ORIENTED_EDGE ( 'NONE', *, *, #10056, .F. ) ;
#2075 = VERTEX_POINT ( 'NONE', #9006 ) ;
#2076 = DIRECTION ( 'NONE',  ( -8.745957808406929547E-15, -2.915319269468972624E-14, 1.000000000000000000 ) ) ;
#2077 = CIRCLE ( 'NONE', #5386, 5.000000000000004441 ) ;
#2078 = AXIS2_PLACEMENT_3D ( 'NONE', #2287, #9161, #10046 ) ;
#2079 = CARTESIAN_POINT ( 'NONE',  ( 636.9746078850427011, 155.6249658629529620, 211.0000000000000000 ) ) ;
#2080 = LINE ( 'NONE', #14564, #5664 ) ;
#2081 = VECTOR ( 'NONE', #9838, 1000.000000000000000 ) ;
#2082 = ORIENTED_EDGE ( 'NONE', *, *, #12974, .F. ) ;
#2083 = ADVANCED_FACE ( 'NONE', ( #10188 ), #47, .T. ) ;
#2084 = ORIENTED_EDGE ( 'NONE', *, *, #5673, .F. ) ;
#2085 = CARTESIAN_POINT ( 'NONE',  ( 0.5219667817988800085, -7.204195837485521281, -0.5602453477493418710 ) ) ;
#2086 = CYLINDRICAL_SURFACE ( 'NONE', #2110, 2.396904916527700102 ) ;
#2087 = CIRCLE ( 'NONE', #13176, 8.331345277524542681 ) ;
#2088 = VECTOR ( 'NONE', #3181, 1000.000000000000000 ) ;
#2089 = CARTESIAN_POINT ( 'NONE',  ( 3.399999999999999911, 0.000000000000000000, -8.000000000000000000 ) ) ;
#2090 = CARTESIAN_POINT ( 'NONE',  ( -2.499999999999999556, 3.061616997868382648E-16, 3.469446951953614189E-15 ) ) ;
#2091 = CARTESIAN_POINT ( 'NONE',  ( 148.9991633467111569, 386.6211705227183870, -187.0000000000000568 ) ) ;
#2092 = SURFACE_STYLE_USAGE ( .BOTH. , #2020 ) ;
#2093 = ORIENTED_EDGE ( 'NONE', *, *, #10269, .F. ) ;
#2094 = DIRECTION ( 'NONE',  ( 0.000000000000000000, -0.8660254037844380415, 0.5000000000000012212 ) ) ;
#2095 = ORIENTED_EDGE ( 'NONE', *, *, #11278, .T. ) ;
#2096 = CARTESIAN_POINT ( 'NONE',  ( -8.505790995054976378, 418.4210031920615052, 190.0000000000000000 ) ) ;
#2097 = AXIS2_PLACEMENT_3D ( 'NONE', #9208, #1237, #3527 ) ;
#2098 = ORIENTED_EDGE ( 'NONE', *, *, #2675, .T. ) ;
#2099 = CIRCLE ( 'NONE', #10360, 5.249999999999976907 ) ;
#2100 = DIRECTION ( 'NONE',  ( 0.000000000000000000, 1.000000000000000000, 0.000000000000000000 ) ) ;
#2101 = EDGE_CURVE ( 'NONE', #5202, #734, #12179, .T. ) ;
#2102 = PLANE ( 'NONE',  #8269 ) ;
#2103 = ORIENTED_EDGE ( 'NONE', *, *, #9085, .F. ) ;
#2104 = CARTESIAN_POINT ( 'NONE',  ( 1.250000000000000000, -6.429618962271402616, -1.000000000000000000 ) ) ;
#2105 = DIRECTION ( 'NONE',  ( 0.8191520442889902442, 1.003171929053522651E-16, -0.5735764363510482688 ) ) ;
#2106 = CIRCLE ( 'NONE', #7547, 20.00000000000001776 ) ;
#2107 = DIRECTION ( 'NONE',  ( -0.2873478855663396114, -0.9578262852211530953, 0.000000000000000000 ) ) ;
#2108 = VERTEX_POINT ( 'NONE', #6933 ) ;
#2109 = AXIS2_PLACEMENT_3D ( 'NONE', #7802, #10011, #8684 ) ;
#2110 = AXIS2_PLACEMENT_3D ( 'NONE', #11105, #14501, #6894 ) ;
#2111 = PRESENTATION_STYLE_ASSIGNMENT (( #13412 ) ) ;
#2112 = ORIENTED_EDGE ( 'NONE', *, *, #12312, .T. ) ;
#2113 = VERTEX_POINT ( 'NONE', #11428 ) ;
#2115 = PLANE ( 'NONE',  #2547 ) ;
#2114 = CIRCLE ( 'NONE', #6136, 2.500000000000000888 ) ;
#2116 = AXIS2_PLACEMENT_3D ( 'NONE', #8413, #3866, #12925 ) ;
#2117 = CARTESIAN_POINT ( 'NONE',  ( 633.0482295921264040, 152.6904006748949030, -210.0000000000000000 ) ) ;
#2118 = EDGE_CURVE ( 'NONE', #7440, #5405, #12913, .T. ) ;
#2120 = CIRCLE ( 'NONE', #1659, 4.000000000000000000 ) ;
#2119 = CARTESIAN_POINT ( 'NONE',  ( 4.000000000000000000, -2.309401076758516691, -0.4999999999999995559 ) ) ;
#2121 = DIRECTION ( 'NONE',  ( 1.000000000000000000, 0.000000000000000000, 0.000000000000000000 ) ) ;
#2122 = EDGE_CURVE ( 'NONE', #173, #4517, #6550, .T. ) ;
#2123 = CARTESIAN_POINT ( 'NONE',  ( 1.863472483959459822E-17, 0.3911686820828793598, -4.000000000000000000 ) ) ;
#2124 = DIRECTION ( 'NONE',  ( 0.000000000000000000, 0.000000000000000000, -1.000000000000000000 ) ) ;
#2125 = VECTOR ( 'NONE', #7691, 1000.000000000000000 ) ;
#2126 = FACE_OUTER_BOUND ( 'NONE', #7480, .T. ) ;
#2127 = EDGE_CURVE ( 'NONE', #3628, #7440, #8172, .T. ) ;
#2128 = EDGE_LOOP ( 'NONE', ( #10320, #2717, #14381, #1494, #3706, #8597, #10276 ) ) ;
#2129 = CIRCLE ( 'NONE', #12989, 2.700000000000000622 ) ;
#2130 = EDGE_CURVE ( 'NONE', #7506, #3336, #2792, .T. ) ;
#2131 = CARTESIAN_POINT ( 'NONE',  ( 6.196878017913830305, 1.924500897298746738, -4.999999999999999112 ) ) ;
#2132 = DIRECTION ( 'NONE',  ( 1.000000000000000000, 0.000000000000000000, 0.000000000000000000 ) ) ;
#2133 = APPLICATION_PROTOCOL_DEFINITION ( 'draft international standard', 'automotive_design', 1998, #2246 ) ;
#2134 = CIRCLE ( 'NONE', #13699, 3.399999999999999911 ) ;
#2136 = EDGE_CURVE ( 'NONE', #9276, #4023, #8328, .T. ) ;
#2135 = CARTESIAN_POINT ( 'NONE',  ( 6.500000000000000000, 3.752776749732563921, -6.064240316920399110 ) ) ;
#2137 = ORIENTED_EDGE ( 'NONE', *, *, #7550, .F. ) ;
#2138 = EDGE_LOOP ( 'NONE', ( #117, #4853, #8394, #887 ) ) ;
#2139 = CARTESIAN_POINT ( 'NONE',  ( 0.000000000000000000, 0.000000000000000000, -8.000000000000000000 ) ) ;
#2140 = CARTESIAN_POINT ( 'NONE',  ( -111.4713065522750952, 33.44139196568231398, 190.0000000000000000 ) ) ;
#2141 = CARTESIAN_POINT ( 'NONE',  ( 629.0000000000000000, 154.0000000000000284, -187.5000000000000000 ) ) ;
#2142 = AXIS2_PLACEMENT_3D ( 'NONE', #6346, #7746, #2121 ) ;
#2143 = AXIS2_PLACEMENT_3D ( 'NONE', #9097, #2226, #2158 ) ;
#2144 = CARTESIAN_POINT ( 'NONE',  ( -6.878751942472531411, 3.924677726130923361, -6.573129608219089981 ) ) ;
#2145 = AXIS2_PLACEMENT_3D ( 'NONE', #6253, #9657, #13055 ) ;
#2146 = VERTEX_POINT ( 'NONE', #4812 ) ;
#2147 = PRESENTATION_LAYER_ASSIGNMENT (  '', '', ( #6640 ) ) ;
#2148 = CARTESIAN_POINT ( 'NONE',  ( 33.50000000000000000, 0.000000000000000000, 2.054999999999999716 ) ) ;
#2149 = ORIENTED_EDGE ( 'NONE', *, *, #13921, .T. ) ;
#2150 = EDGE_CURVE ( 'NONE', #4953, #5257, #7720, .T. ) ;
#2151 = EDGE_CURVE ( 'NONE', #5281, #6413, #9447, .T. ) ;
#2152 = DIRECTION ( 'NONE',  ( -0.000000000000000000, -0.000000000000000000, -1.000000000000000000 ) ) ;
#2153 = CARTESIAN_POINT ( 'NONE',  ( 2.354826896168714434, -6.962563485461402024, -1.000000000000000000 ) ) ;
#2154 = CIRCLE ( 'NONE', #12535, 2.199999999999988187 ) ;
#2155 = LINE ( 'NONE', #12566, #8727 ) ;
#2156 = ORIENTED_EDGE ( 'NONE', *, *, #13907, .F. ) ;
#2157 = ORIENTED_EDGE ( 'NONE', *, *, #4058, .T. ) ;
#2158 = DIRECTION ( 'NONE',  ( -1.000000000000000000, 0.000000000000000000, 0.000000000000000000 ) ) ;
#2159 =( GEOMETRIC_REPRESENTATION_CONTEXT ( 3 ) GLOBAL_UNCERTAINTY_ASSIGNED_CONTEXT ( ( #2667 ) ) GLOBAL_UNIT_ASSIGNED_CONTEXT ( ( #14207, #11009, #13162 ) ) REPRESENTATION_CONTEXT ( 'NONE', 'WORKASPACE' ) );
#2160 = DIRECTION ( 'NONE',  ( -1.000000000000000000, 0.000000000000000000, 0.000000000000000000 ) ) ;
#2161 = EDGE_CURVE ( 'NONE', #10356, #7765, #6200, .T. ) ;
#2162 = CARTESIAN_POINT ( 'NONE',  ( -2.100000000000000089, 2.571758278209441957E-16, -0.2800830152838844622 ) ) ;
#2163 = TOROIDAL_SURFACE ( 'NONE', #10671, 5.100000000000000533, 0.1000000000000001582 ) ;
#2164 = EDGE_CURVE ( 'NONE', #3784, #2958, #10926, .T. ) ;
#2165 = VERTEX_POINT ( 'NONE', #10406 ) ;
#2166 = ORIENTED_EDGE ( 'NONE', *, *, #9445, .T. ) ;
#2167 = FACE_OUTER_BOUND ( 'NONE', #3892, .T. ) ;
#2168 =( REPRESENTATION_RELATIONSHIP ('NONE','NONE', #2822, #5462 ) REPRESENTATION_RELATIONSHIP_WITH_TRANSFORMATION ( #14509 )SHAPE_REPRESENTATION_RELATIONSHIP( ) );
#2169 = FACE_OUTER_BOUND ( 'NONE', #5104, .T. ) ;
#2170 = MANIFOLD_SOLID_BREP ( 'OuterRace', #9516 ) ;
#2171 = LINE ( 'NONE', #6533, #3024 ) ;
#2172 = CARTESIAN_POINT ( 'NONE',  ( -0.1481481481481481122, -4.797713218419819903, -1.000000000000000000 ) ) ;
#2173 =( NAMED_UNIT ( * ) PLANE_ANGLE_UNIT ( ) SI_UNIT ( $, .RADIAN. ) );
#2174 = ORIENTED_EDGE ( 'NONE', *, *, #4397, .F. ) ;
#2175 = B_SPLINE_CURVE_WITH_KNOTS ( 'NONE', 3,
 ( #9844, #5345, #14346, #7779, #5495, #11094, #12055, #14279 ),
 .UNSPECIFIED., .F., .F.,
 ( 4, 2, 2, 4 ),
 ( 0.002921158011986723334, 0.003648658599403076588, 0.004376159186819428976, 0.005831160361652135485 ),
 .UNSPECIFIED. ) ;
#2176 = CARTESIAN_POINT ( 'NONE',  ( 10.00000000000000000, 0.000000000000000000, -210.0000000000000000 ) ) ;
#2177 = ORIENTED_EDGE ( 'NONE', *, *, #1917, .F. ) ;
#2178 = ORIENTED_EDGE ( 'NONE', *, *, #14231, .F. ) ;
#2179 = AXIS2_PLACEMENT_3D ( 'NONE', #7051, #11556, #1455 ) ;
#2180 = FACE_OUTER_BOUND ( 'NONE', #10813, .T. ) ;
#2181 = VECTOR ( 'NONE', #8424, 1000.000000000000000 ) ;
#2182 = ORIENTED_EDGE ( 'NONE', *, *, #4749, .F. ) ;
#2183 = DIRECTION ( 'NONE',  ( 1.000000000000000000, 0.000000000000000000, 0.000000000000000000 ) ) ;
#2184 = LINE ( 'NONE', #11038, #10409 ) ;
#2185 = CIRCLE ( 'NONE', #2668, 2.649999999999985700 ) ;
#2186 = EDGE_LOOP ( 'NONE', ( #11729, #3232, #3231, #11948, #2256, #7091, #1090, #687 ) ) ;
#2187 = DIRECTION ( 'NONE',  ( -1.000000000000000000, 0.000000000000000000, 0.000000000000000000 ) ) ;
#2188 = DIRECTION ( 'NONE',  ( 1.000000000000000000, 0.000000000000000000, 0.000000000000000000 ) ) ;
#2189 = CARTESIAN_POINT ( 'NONE',  ( 6.196878017913830305, -1.924500897298746072, 4.999999999999999112 ) ) ;
#2190 = DIRECTION ( 'NONE',  ( 0.2873478855663497700, 0.9578262852211499867, 5.078292077360263497E-30 ) ) ;
#2191 = FILL_AREA_STYLE_COLOUR ( '', #11800 ) ;
#2192 = ORIENTED_EDGE ( 'NONE', *, *, #7150, .F. ) ;
#2193 = LINE ( 'NONE', #8778, #9880 ) ;
#2194 = ORIENTED_EDGE ( 'NONE', *, *, #12145, .F. ) ;
#2195 = ADVANCED_FACE ( 'NONE', ( #1478 ), #10477, .F. ) ;
#2196 = EDGE_LOOP ( 'NONE', ( #11046, #14061, #1815, #7159 ) ) ;
#2197 = DIRECTION ( 'NONE',  ( -1.000000000000000000, 0.000000000000000000, 0.000000000000000000 ) ) ;
#2198 = FACE_BOUND ( 'NONE', #8661, .T. ) ;
#2199 = LINE ( 'NONE', #10024, #241 ) ;
#2200 = CARTESIAN_POINT ( 'NONE',  ( 604.3113219698376497, -181.2933965909545861, -149.9999999999986642 ) ) ;
#2201 = FACE_OUTER_BOUND ( 'NONE', #14284, .T. ) ;
#2202 = DIRECTION ( 'NONE',  ( -1.000000000000000000, 0.000000000000000000, 0.000000000000000000 ) ) ;
#2203 = LINE ( 'NONE', #6930, #324 ) ;
#2204 = ORIENTED_EDGE ( 'NONE', *, *, #7111, .F. ) ;
#2205 = DIRECTION ( 'NONE',  ( 0.000000000000000000, 0.000000000000000000, 1.000000000000000000 ) ) ;
#2206 = PLANE ( 'NONE',  #6110 ) ;
#2207 = EDGE_CURVE ( 'NONE', #9473, #1845, #8475, .T. ) ;
#2208 = CARTESIAN_POINT ( 'NONE',  ( -2.059999999999998721, 2.522772406243545965E-16, -0.3080913168122742518 ) ) ;
#2209 = EDGE_LOOP ( 'NONE', ( #9368, #6756, #10801, #13263, #4741 ) ) ;
#2210 = ORIENTED_EDGE ( 'NONE', *, *, #2498, .T. ) ;
#2211 = CARTESIAN_POINT ( 'NONE',  ( 237.7887055630606028, 337.0156335382089310, -179.8000000000007219 ) ) ;
#2212 = ADVANCED_FACE ( 'NONE', ( #12908 ), #7156, .F. ) ;
#2213 = CARTESIAN_POINT ( 'NONE',  ( 610.0000000000000000, 227.4403065089105951, 187.0000000000000000 ) ) ;
#2214 = EDGE_CURVE ( 'NONE', #1456, #4552, #1694, .T. ) ;
#2215 = MANIFOLD_SOLID_BREP ( 'Hex', #7630 ) ;
#2216 = DIRECTION ( 'NONE',  ( 0.000000000000000000, 1.000000000000000000, -1.224646799147353207E-16 ) ) ;
#2217 = VERTEX_POINT ( 'NONE', #7442 ) ;
#2218 = EDGE_CURVE ( 'NONE', #11861, #4517, #3980, .T. ) ;
#2219 = DIRECTION ( 'NONE',  ( 0.9578262852211513190, -0.2873478855663453291, 0.000000000000000000 ) ) ;
#2220 = ORIENTED_EDGE ( 'NONE', *, *, #11012, .T. ) ;
#2221 = CARTESIAN_POINT ( 'NONE',  ( 21.00000000000000355, 0.000000000000000000, 0.000000000000000000 ) ) ;
#2222 = PLANE ( 'NONE',  #663 ) ;
#2223 = DIRECTION ( 'NONE',  ( -0.000000000000000000, -0.000000000000000000, 1.000000000000000000 ) ) ;
#2224 = VERTEX_POINT ( 'NONE', #7599 ) ;
#2225 = VERTEX_POINT ( 'NONE', #1981 ) ;
#2226 = DIRECTION ( 'NONE',  ( -0.000000000000000000, -0.000000000000000000, -1.000000000000000000 ) ) ;
#2227 = CARTESIAN_POINT ( 'NONE',  ( 637.5000000000000000, 160.0000000000000284, -217.5000000000000284 ) ) ;
#2228 = EDGE_CURVE ( 'NONE', #1307, #3448, #11946, .T. ) ;
#2229 = EDGE_CURVE ( 'NONE', #10293, #1652, #14305, .T. ) ;
#2230 = FACE_OUTER_BOUND ( 'NONE', #4194, .T. ) ;
#2231 = EDGE_LOOP ( 'NONE', ( #10930, #68 ) ) ;
#2232 = EDGE_CURVE ( 'NONE', #2113, #4509, #4937, .T. ) ;
#2233 = ORIENTED_EDGE ( 'NONE', *, *, #8909, .T. ) ;
#2234 = DIRECTION ( 'NONE',  ( 0.000000000000000000, 1.000000000000000000, 0.000000000000000000 ) ) ;
#2235 = CARTESIAN_POINT ( 'NONE',  ( 1.654252653721905331, 3.663718938583014229, -0.01223254789873410957 ) ) ;
#2236 = CARTESIAN_POINT ( 'NONE',  ( 0.1404048886732821022, 4.699864953788070565, -3.686887068327037387 ) ) ;
#2237 = CARTESIAN_POINT ( 'NONE',  ( 446.3084422793565409, 264.0194060144110608, 210.0000000000000000 ) ) ;
#2238 =( NAMED_UNIT ( * ) PLANE_ANGLE_UNIT ( ) SI_UNIT ( $, .RADIAN. ) );
#2239 = ORIENTED_EDGE ( 'NONE', *, *, #13792, .F. ) ;
#2240 = FACE_OUTER_BOUND ( 'NONE', #10042, .T. ) ;
#2241 = ORIENTED_EDGE ( 'NONE', *, *, #8930, .T. ) ;
#2242 = VERTEX_POINT ( 'NONE', #9805 ) ;
#2243 = CARTESIAN_POINT ( 'NONE',  ( 6.242811304425486263, -0.9953138271156629635, -5.105233480330447549 ) ) ;
#2244 = ORIENTED_EDGE ( 'NONE', *, *, #504, .T. ) ;
#2245 = DIRECTION ( 'NONE',  ( -0.000000000000000000, -0.000000000000000000, 1.000000000000000000 ) ) ;
#2246 = APPLICATION_CONTEXT ( 'automotive_design' ) ;
#2247 = CARTESIAN_POINT ( 'NONE',  ( 0.1481481481481481122, -4.797713218419819903, -1.000000000000000000 ) ) ;
#2248 = SHAPE_REPRESENTATION ( 'stationary channel', ( #9440 ), #8508 ) ;
#2249 = ORIENTED_EDGE ( 'NONE', *, *, #10270, .F. ) ;
#2250 = CARTESIAN_POINT ( 'NONE',  ( 139.8040310085880833, 355.9707293956415697, 190.0000000000000000 ) ) ;
#2251 = DIRECTION ( 'NONE',  ( -0.4113766427172327877, 0.9114654452181378819, 0.000000000000000000 ) ) ;
#2252 = CARTESIAN_POINT ( 'NONE',  ( -1.049032378834002577, -6.899894373156699068, -0.3607371497494579748 ) ) ;
#2253 = LINE ( 'NONE', #13712, #1951 ) ;
#2254 = EDGE_LOOP ( 'NONE', ( #8971, #12568, #816, #1418 ) ) ;
#2255 = CARTESIAN_POINT ( 'NONE',  ( 1.600000000000000089, 0.000000000000000000, 2.700000000000000178 ) ) ;
#2256 = ORIENTED_EDGE ( 'NONE', *, *, #2297, .F. ) ;
#2257 = EDGE_LOOP ( 'NONE', ( #9149, #722, #9505, #994 ) ) ;
#2258 = CARTESIAN_POINT ( 'NONE',  ( 237.7887055630605460, 337.0156335382089310, -179.8000000000007219 ) ) ;
#2259 = PRODUCT_DEFINITION_SHAPE ( 'NONE', 'NONE',  #11257 ) ;
#2260 = DIRECTION ( 'NONE',  ( 0.000000000000000000, -1.000000000000000000, 0.000000000000000000 ) ) ;
#2261 = CARTESIAN_POINT ( 'NONE',  ( -9.137956343300997375, 374.5525593289318635, 169.9999999999999716 ) ) ;
#2262 = ADVANCED_FACE ( 'NONE', ( #10592 ), #14138, .T. ) ;
#2263 = CARTESIAN_POINT ( 'NONE',  ( 137.1540310085880776, 355.9707293956415697, 187.0000000000000000 ) ) ;
#2264 = EDGE_CURVE ( 'NONE', #14524, #1319, #13839, .T. ) ;
#2265 = CARTESIAN_POINT ( 'NONE',  ( 610.0000000000001137, 191.1080398579018720, -187.0000000000000000 ) ) ;
#2266 = DIRECTION ( 'NONE',  ( 0.000000000000000000, 0.000000000000000000, 1.000000000000000000 ) ) ;
#2267 = DIRECTION ( 'NONE',  ( 0.000000000000000000, 0.000000000000000000, 1.000000000000000000 ) ) ;
#2268 = VERTEX_POINT ( 'NONE', #1799 ) ;
#2269 = CARTESIAN_POINT ( 'NONE',  ( -4.444974277458378253, -4.939246403833585042, -5.720331885005373707 ) ) ;
#2270 = CARTESIAN_POINT ( 'NONE',  ( 6.481779955677548166, -5.820445026626441809, 3.602012395189916580E-16 ) ) ;
#2271 = VERTEX_POINT ( 'NONE', #11908 ) ;
#2272 = AXIS2_PLACEMENT_3D ( 'NONE', #11062, #14534, #11281 ) ;
#2273 = CARTESIAN_POINT ( 'NONE',  ( 6.663127973346361976, 3.846958729056444426, -6.460793508093577664 ) ) ;
#2274 = ORIENTED_EDGE ( 'NONE', *, *, #942, .T. ) ;
#2275 = ORIENTED_EDGE ( 'NONE', *, *, #9049, .T. ) ;
#2276 = PLANE ( 'NONE',  #12484 ) ;
#2277 = AXIS2_PLACEMENT_3D ( 'NONE', #948, #6650, #11942 ) ;
#2279 = DIRECTION ( 'NONE',  ( 1.000000000000000000, 0.000000000000000000, 0.000000000000000000 ) ) ;
#2278 = CIRCLE ( 'NONE', #10307, 5.000000000000004441 ) ;
#2280 = ADVANCED_FACE ( 'NONE', ( #6175 ), #3739, .F. ) ;
#2281 = LINE ( 'NONE', #8788, #13228 ) ;
#2282 = CARTESIAN_POINT ( 'NONE',  ( 153.1991633467111456, 386.6211705227183870, -210.0000000000000000 ) ) ;
#2283 = ORIENTED_EDGE ( 'NONE', *, *, #8961, .F. ) ;
#2284 = VECTOR ( 'NONE', #2575, 1000.000000000000000 ) ;
#2285 = AXIS2_PLACEMENT_3D ( 'NONE', #2392, #8964, #7790 ) ;
#2286 = FACE_OUTER_BOUND ( 'NONE', #2024, .T. ) ;
#2287 = CARTESIAN_POINT ( 'NONE',  ( 455.5035746174796714, 294.6698471414878782, 210.0000000000000000 ) ) ;
#2288 = EDGE_CURVE ( 'NONE', #12648, #9517, #610, .T. ) ;
#2289 = PLANE ( 'NONE',  #4257 ) ;
#2290 = VERTEX_POINT ( 'NONE', #2764 ) ;
#2291 = VERTEX_POINT ( 'NONE', #12735 ) ;
#2292 = DIRECTION ( 'NONE',  ( 0.000000000000000000, 0.000000000000000000, -1.000000000000000000 ) ) ;
#2293 = FACE_OUTER_BOUND ( 'NONE', #7234, .T. ) ;
#2294 = AXIS2_PLACEMENT_3D ( 'NONE', #14046, #7317, #14110 ) ;
#2295 = DIRECTION ( 'NONE',  ( 1.501925087425806625E-16, 4.055197736049677764E-15, 1.000000000000000000 ) ) ;
#2296 = CIRCLE ( 'NONE', #12436, 2.500000000000000444 ) ;
#2297 = EDGE_CURVE ( 'NONE', #4638, #8007, #1581, .T. ) ;
#2298 = VERTEX_POINT ( 'NONE', #2700 ) ;
#2299 = ORIENTED_EDGE ( 'NONE', *, *, #8745, .T. ) ;
#2300 = CARTESIAN_POINT ( 'NONE',  ( 610.0000000000001137, 191.1080398579019288, -190.0000000000000284 ) ) ;
#2301 = PLANE ( 'NONE',  #12720 ) ;
#2302 = CARTESIAN_POINT ( 'NONE',  ( 6.385552186430389021, 5.773502691896261751, 0.000000000000000000 ) ) ;
#2303 = CYLINDRICAL_SURFACE ( 'NONE', #2285, 2.499999999999946709 ) ;
#2304 = DIRECTION ( 'NONE',  ( -0.000000000000000000, -0.000000000000000000, 1.000000000000000000 ) ) ;
#2305 = PRESENTATION_STYLE_ASSIGNMENT (( #1288 ) ) ;
#2306 = B_SPLINE_CURVE_WITH_KNOTS ( 'NONE', 3,
 ( #11439, #10765, #13130, #14309, #9749, #798 ),
 .UNSPECIFIED., .F., .F.,
 ( 4, 2, 4 ),
 ( 8.673617379884035472E-19, 0.0003352299596267603100, 0.0006704599192535197526 ),
 .UNSPECIFIED. ) ;
#2307 = EDGE_CURVE ( 'NONE', #10292, #10447, #314, .T. ) ;
#2308 = EDGE_LOOP ( 'NONE', ( #3923, #3714, #6296, #3982 ) ) ;
#2309 = MECHANICAL_DESIGN_GEOMETRIC_PRESENTATION_REPRESENTATION (  '', ( #651 ), #10568 ) ;
#2310 = EDGE_CURVE ( 'NONE', #8377, #72, #7268, .T. ) ;
#2311 = CARTESIAN_POINT ( 'NONE',  ( 703.1581845006096501, 166.2926764603917036, -177.6000000000005059 ) ) ;
#2312 = AXIS2_PLACEMENT_3D ( 'NONE', #7015, #12474, #288 ) ;
#2313 = ORIENTED_EDGE ( 'NONE', *, *, #13602, .F. ) ;
#2314 = VERTEX_POINT ( 'NONE', #4851 ) ;
#2315 = CARTESIAN_POINT ( 'NONE',  ( 632.5000000000001137, 160.0000000000000284, -233.5000000000000000 ) ) ;
#2316 = ADVANCED_FACE ( 'NONE', ( #2634 ), #7200, .T. ) ;
#2317 = EDGE_LOOP ( 'NONE', ( #855, #1800, #4859, #11102 ) ) ;
#2318 = DIRECTION ( 'NONE',  ( -0.2873478855663446629, -0.9578262852211516520, -5.337610695313252962E-15 ) ) ;
#2319 = DIRECTION ( 'NONE',  ( 1.000000000000000000, -3.469446951953611033E-15, -0.000000000000000000 ) ) ;
#2320 = VECTOR ( 'NONE', #13632, 1000.000000000000227 ) ;
#2321 = AXIS2_PLACEMENT_3D ( 'NONE', #7580, #10903, #9790 ) ;
#2322 = ORIENTED_EDGE ( 'NONE', *, *, #1223, .T. ) ;
#2323 = CARTESIAN_POINT ( 'NONE',  ( 1.500000000000001332, 0.000000000000000000, 0.000000000000000000 ) ) ;
#2324 = CARTESIAN_POINT ( 'NONE',  ( 20.55500000000001748, 0.000000000000000000, 0.000000000000000000 ) ) ;
#2325 = CARTESIAN_POINT ( 'NONE',  ( -122.9652219749294488, 36.88956659247806869, -189.9999999999986358 ) ) ;
#2326 = CARTESIAN_POINT ( 'NONE',  ( -2.688821387764050996E-14, -4.618802153517012954, -0.4999999999999995559 ) ) ;
#2327 = SURFACE_STYLE_FILL_AREA ( #10166 ) ;
#2328 = VERTEX_POINT ( 'NONE', #1663 ) ;
#2329 = VECTOR ( 'NONE', #2494, 1000.000000000000000 ) ;
#2330 = CARTESIAN_POINT ( 'NONE',  ( 0.03421028094653320167, 3.855830693249143515, 1.321505333908966184 ) ) ;
#2331 = ORIENTED_EDGE ( 'NONE', *, *, #11098, .T. ) ;
#2332 = AXIS2_PLACEMENT_3D ( 'NONE', #201, #9308, #13809 ) ;
#2333 = TOROIDAL_SURFACE ( 'NONE', #12469, 5.384454397937118664, 0.5155456020628804703 ) ;
#2334 = ORIENTED_EDGE ( 'NONE', *, *, #14098, .T. ) ;
#2335 = CARTESIAN_POINT ( 'NONE',  ( -9.511508594537124495, 378.5275384125996538, 187.0000000000000284 ) ) ;
#2336 = ADVANCED_FACE ( 'NONE', ( #8304 ), #4032, .F. ) ;
#2337 = CARTESIAN_POINT ( 'NONE',  ( 164.3243839102495656, 402.9042173714779551, -190.0000000000000000 ) ) ;
#2338 = B_SPLINE_CURVE_WITH_KNOTS ( 'NONE', 3,
 ( #13810, #1406, #9240, #10419, #10118, #8185 ),
 .UNSPECIFIED., .F., .F.,
 ( 4, 2, 4 ),
 ( 0.006655250997664721377, 0.007825277639709776745, 0.008995304281754830378 ),
 .UNSPECIFIED. ) ;
#2339 =( GEOMETRIC_REPRESENTATION_CONTEXT ( 3 ) GLOBAL_UNCERTAINTY_ASSIGNED_CONTEXT ( ( #127 ) ) GLOBAL_UNIT_ASSIGNED_CONTEXT ( ( #3308, #11048, #11129 ) ) REPRESENTATION_CONTEXT ( 'NONE', 'WORKASPACE' ) );
#2340 = CARTESIAN_POINT ( 'NONE',  ( 2.999999999999999112, 0.000000000000000000, -4.000000000000000000 ) ) ;
#2341 = ADVANCED_FACE ( 'NONE', ( #384 ), #12881, .F. ) ;
#2342 = PLANE ( 'NONE',  #11572 ) ;
#2343 = VECTOR ( 'NONE', #10076, 1000.000000000000000 ) ;
#2344 = ADVANCED_FACE ( 'NONE', ( #2845 ), #12814, .F. ) ;
#2345 = CONICAL_SURFACE ( 'NONE', #12249, 2.500000000000000888, 0.9599310885968785900 ) ;
#2346 = DIRECTION ( 'NONE',  ( 0.000000000000000000, 1.000000000000000000, -1.224646799147353207E-16 ) ) ;
#2347 = DIRECTION ( 'NONE',  ( -0.7071067811865530128, 8.659560562354868763E-17, -0.7071067811865421326 ) ) ;
#2348 = CARTESIAN_POINT ( 'NONE',  ( 112.9652219749295483, 376.5507399164318372, 1.650218294979717018E-14 ) ) ;
#2349 = ORIENTED_EDGE ( 'NONE', *, *, #4390, .F. ) ;
#2350 = DIRECTION ( 'NONE',  ( -0.2873478855663477716, -0.9578262852211506528, 0.000000000000000000 ) ) ;
#2351 = CARTESIAN_POINT ( 'NONE',  ( 7.336184427528458230, 0.000000000000000000, -8.105212085995399107 ) ) ;
#2352 = APPLICATION_PROTOCOL_DEFINITION ( 'draft international standard', 'automotive_design', 1998, #2533 ) ;
#2353 = EDGE_LOOP ( 'NONE', ( #10857, #13525, #680, #9937 ) ) ;
#2354 = CIRCLE ( 'NONE', #8012, 4.199999999999981526 ) ;
#2355 = AXIS2_PLACEMENT_3D ( 'NONE', #12339, #8060, #4378 ) ;
#2356 = B_SPLINE_CURVE_WITH_KNOTS ( 'NONE', 3,
 ( #4320, #69, #4610, #3355, #11234, #3420, #6886, #7920 ),
 .UNSPECIFIED., .F., .F.,
 ( 4, 2, 2, 4 ),
 ( 0.000000000000000000, 0.002450665683189820997, 0.003675998524784731495, 0.004901331366379641993 ),
 .UNSPECIFIED. ) ;
#2357 = PLANE ( 'NONE',  #6612 ) ;
#2358 = VERTEX_POINT ( 'NONE', #14005 ) ;
#2359 = ORIENTED_EDGE ( 'NONE', *, *, #1975, .T. ) ;
#2360 = DIRECTION ( 'NONE',  ( 1.000000000000000000, 0.000000000000000000, 0.000000000000000000 ) ) ;
#2361 = AXIS2_PLACEMENT_3D ( 'NONE', #13330, #11036, #921 ) ;
#2362 = CIRCLE ( 'NONE', #10864, 5.000000000000004441 ) ;
#2363 = EDGE_CURVE ( 'NONE', #1120, #13126, #13051, .T. ) ;
#2364 = CARTESIAN_POINT ( 'NONE',  ( 5.560781378645573980, 6.809993116116507654E-16, -4.000000000000000000 ) ) ;
#2365 = VECTOR ( 'NONE', #1764, 1000.000000000000000 ) ;
#2366 = DIRECTION ( 'NONE',  ( -0.000000000000000000, -0.000000000000000000, -1.000000000000000000 ) ) ;
#2367 = CIRCLE ( 'NONE', #1424, 4.250000000000000000 ) ;
#2368 = CARTESIAN_POINT ( 'NONE',  ( 6.507056315241516842, -5.826803161468475878, 0.09231912136634906618 ) ) ;
#2369 = VERTEX_POINT ( 'NONE', #8440 ) ;
#2370 = AXIS2_PLACEMENT_3D ( 'NONE', #13791, #11566, #1467 ) ;
#2371 = LINE ( 'NONE', #11516, #898 ) ;
#2372 = CARTESIAN_POINT ( 'NONE',  ( 635.0000000000000000, 160.0000000000000284, 211.0000000000000000 ) ) ;
#2373 =( LENGTH_UNIT ( ) NAMED_UNIT ( * ) SI_UNIT ( .MILLI., .METRE. ) );
#2374 = B_SPLINE_CURVE_WITH_KNOTS ( 'NONE', 3,
 ( #11415, #8023, #2330, #9285, #10169, #11478 ),
 .UNSPECIFIED., .F., .F.,
 ( 4, 2, 4 ),
 ( 0.002336974151641533874, 0.003500975885716431542, 0.004664977619791329209 ),
 .UNSPECIFIED. ) ;
#2375 = CARTESIAN_POINT ( 'NONE',  ( 446.3084422793565409, 264.0194060144110608, 210.0000000000000000 ) ) ;
#2376 = ORIENTED_EDGE ( 'NONE', *, *, #6692, .T. ) ;
#2377 = ORIENTED_EDGE ( 'NONE', *, *, #11620, .F. ) ;
#2378 = VECTOR ( 'NONE', #9459, 1000.000000000000000 ) ;
#2379 = CARTESIAN_POINT ( 'NONE',  ( 701.6639754956653405, 161.3119797772417883, -177.6000000000005059 ) ) ;
#2380 = CARTESIAN_POINT ( 'NONE',  ( -20.63749999999999929, 0.000000000000000000, 0.000000000000000000 ) ) ;
#2381 = ADVANCED_FACE ( 'NONE', ( #1737 ), #9636, .F. ) ;
#2382 = AXIS2_PLACEMENT_3D ( 'NONE', #7418, #8300, #2627 ) ;
#2383 = DIRECTION ( 'NONE',  ( -9.028085479645851510E-15, -3.009361826548617065E-14, 1.000000000000000000 ) ) ;
#2384 = CIRCLE ( 'NONE', #12652, 2.054999999999999716 ) ;
#2385 = CARTESIAN_POINT ( 'NONE',  ( 6.327632967270169217, 5.346704644971289611, -0.7392359018470683329 ) ) ;
#2386 = ORIENTED_EDGE ( 'NONE', *, *, #7087, .T. ) ;
#2387 = AXIS2_PLACEMENT_3D ( 'NONE', #4343, #8838, #3224 ) ;
#2388 = ORIENTED_EDGE ( 'NONE', *, *, #211, .F. ) ;
#2389 = CARTESIAN_POINT ( 'NONE',  ( 3.250000000000003109, -5.629165124598849879, 0.000000000000000000 ) ) ;
#2390 = CARTESIAN_POINT ( 'NONE',  ( -9.498873539028489220E-16, 10.00000000000000000, 210.0000000000000000 ) ) ;
#2391 = CARTESIAN_POINT ( 'NONE',  ( 6.367873360227558344, 5.773502691896261751, 0.000000000000000000 ) ) ;
#2392 = CARTESIAN_POINT ( 'NONE',  ( 635.0000000000000000, 160.0000000000000284, -233.5000000000000000 ) ) ;
#2393 =( LENGTH_UNIT ( ) NAMED_UNIT ( * ) SI_UNIT ( .MILLI., .METRE. ) );
#2394 = PRODUCT ( 'hex flange nut gradea_iso_ISO - 4161 - M5 - N', 'hex flange nut gradea_iso_ISO - 4161 - M5 - N', '', ( #8573 ) ) ;
#2395 = ORIENTED_EDGE ( 'NONE', *, *, #5341, .F. ) ;
#2396 =( GEOMETRIC_REPRESENTATION_CONTEXT ( 3 ) GLOBAL_UNCERTAINTY_ASSIGNED_CONTEXT ( ( #9887 ) ) GLOBAL_UNIT_ASSIGNED_CONTEXT ( ( #4840, #9405, #3729 ) ) REPRESENTATION_CONTEXT ( 'NONE', 'WORKASPACE' ) );
#2397 = CARTESIAN_POINT ( 'NONE',  ( 2.100000000000000089, 0.000000000000000000, -0.2800830152838844622 ) ) ;
#2398 = VERTEX_POINT ( 'NONE', #5265 ) ;
#2399 = ORIENTED_EDGE ( 'NONE', *, *, #3834, .T. ) ;
#2400 = LINE ( 'NONE', #2315, #10872 ) ;
#2401 = EDGE_CURVE ( 'NONE', #13831, #796, #7013, .T. ) ;
#2402 = EDGE_LOOP ( 'NONE', ( #1994, #3074 ) ) ;
#2403 = AXIS2_PLACEMENT_3D ( 'NONE', #10500, #5059, #10437 ) ;
#2404 = ADVANCED_FACE ( 'NONE', ( #5327 ), #1776, .F. ) ;
#2405 = DIRECTION ( 'NONE',  ( -0.000000000000000000, -0.000000000000000000, 1.000000000000000000 ) ) ;
#2406 = DIRECTION ( 'NONE',  ( -9.794481010665704304E-16, -3.264827003555233190E-15, -1.000000000000000000 ) ) ;
#2407 = EDGE_CURVE ( 'NONE', #3959, #8752, #526, .T. ) ;
#2408 = AXIS2_PLACEMENT_3D ( 'NONE', #13750, #8123, #290 ) ;
#2409 = ORIENTED_EDGE ( 'NONE', *, *, #13249, .F. ) ;
#2410 = CARTESIAN_POINT ( 'NONE',  ( 590.0000000000000000, 10.00000000000005507, -210.0000000000000000 ) ) ;
#2411 = FACE_OUTER_BOUND ( 'NONE', #1775, .T. ) ;
#2412 = EDGE_CURVE ( 'NONE', #7278, #12527, #643, .T. ) ;
#2413 = DIRECTION ( 'NONE',  ( 0.2873478855663448850, 0.9578262852211515410, -3.408579461568462910E-15 ) ) ;
#2414 = FILL_AREA_STYLE ('',( #6761 ) ) ;
#2415 = FILL_AREA_STYLE_COLOUR ( '', #3334 ) ;
#2416 = VECTOR ( 'NONE', #6630, 1000.000000000000000 ) ;
#2417 = ORIENTED_EDGE ( 'NONE', *, *, #1510, .F. ) ;
#2418 = CARTESIAN_POINT ( 'NONE',  ( 5.991014884144047592, -4.330127018922192761, 2.499999999999998668 ) ) ;
#2419 = ORIENTED_EDGE ( 'NONE', *, *, #3611, .T. ) ;
#2420 = ORIENTED_EDGE ( 'NONE', *, *, #8101, .T. ) ;
#2421 = EDGE_LOOP ( 'NONE', ( #9229, #7654, #3804, #9012 ) ) ;
#2422 = FACE_OUTER_BOUND ( 'NONE', #12765, .T. ) ;
#2423 = CARTESIAN_POINT ( 'NONE',  ( 703.1581845006096501, 166.2926764603917036, 150.0000000000013927 ) ) ;
#2424 =( GEOMETRIC_REPRESENTATION_CONTEXT ( 3 ) GLOBAL_UNCERTAINTY_ASSIGNED_CONTEXT ( ( #13447 ) ) GLOBAL_UNIT_ASSIGNED_CONTEXT ( ( #2705, #7205, #13845 ) ) REPRESENTATION_CONTEXT ( 'NONE', 'WORKASPACE' ) );
#2425 = EDGE_CURVE ( 'NONE', #293, #556, #406, .T. ) ;
#2426 = LINE ( 'NONE', #9290, #726 ) ;
#2427 = EDGE_CURVE ( 'NONE', #7561, #9391, #14094, .T. ) ;
#2428 = DIRECTION ( 'NONE',  ( 0.2873478855663454401, 0.9578262852211513190, 0.000000000000000000 ) ) ;
#2429 = EDGE_CURVE ( 'NONE', #7308, #13410, #10782, .T. ) ;
#2430 = CARTESIAN_POINT ( 'NONE',  ( -1.716263591756835415E-13, -1.266779246227765552E-12, -179.7999999999981355 ) ) ;
#2431 = CYLINDRICAL_SURFACE ( 'NONE', #7085, 4.799999999999968736 ) ;
#2432 = LINE ( 'NONE', #45, #11930 ) ;
#2433 = VERTEX_POINT ( 'NONE', #2967 ) ;
#2434 = DIRECTION ( 'NONE',  ( -0.000000000000000000, -0.000000000000000000, 1.000000000000000000 ) ) ;
#2435 = DIRECTION ( 'NONE',  ( -1.000000000000000000, -0.000000000000000000, -0.000000000000000000 ) ) ;
#2436 = CARTESIAN_POINT ( 'NONE',  ( 610.4468987511024807, 188.9818594558784355, 185.9044171606945497 ) ) ;
#2437 = ITEM_DEFINED_TRANSFORMATION ( 'NONE', 'NONE', #9730,  #9440 ) ;
#2438 = ORIENTED_EDGE ( 'NONE', *, *, #10439, .T. ) ;
#2439 = CLOSED_SHELL ( 'NONE', ( #8354, #13277, #14507, #10352, #2195, #243, #12766, #10082, #1713, #5998, #10469, #5380 ) ) ;
#2440 = VERTEX_POINT ( 'NONE', #6442 ) ;
#2441 = VERTEX_POINT ( 'NONE', #14329 ) ;
#2442 = DIRECTION ( 'NONE',  ( 1.000000000000000000, 0.000000000000000000, 0.000000000000000000 ) ) ;
#2443 = DIRECTION ( 'NONE',  ( -0.000000000000000000, -0.000000000000000000, 1.000000000000000000 ) ) ;
#2444 = CARTESIAN_POINT ( 'NONE',  ( 627.5000000000000000, 160.0000000000000284, 210.0000059999999849 ) ) ;
#2445 = FACE_OUTER_BOUND ( 'NONE', #903, .T. ) ;
#2446 = VERTEX_POINT ( 'NONE', #4087 ) ;
#2447 = PLANE ( 'NONE',  #10533 ) ;
#2448 = DIRECTION ( 'NONE',  ( -0.9237280213470676626, -0.3830490080632388272, 0.000000000000000000 ) ) ;
#2449 = DIRECTION ( 'NONE',  ( 0.000000000000000000, 0.000000000000000000, 1.000000000000000000 ) ) ;
#2450 = DIRECTION ( 'NONE',  ( 0.3543563944859323134, -0.9351104457158685435, 0.000000000000000000 ) ) ;
#2451 = EDGE_LOOP ( 'NONE', ( #14230, #8899, #11648 ) ) ;
#2452 = VERTEX_POINT ( 'NONE', #12928 ) ;
#2453 = LINE ( 'NONE', #13895, #2762 ) ;
#2454 = CARTESIAN_POINT ( 'NONE',  ( 133.6739427831727767, 370.3381236739588189, 190.0000000000000000 ) ) ;
#2455 = CARTESIAN_POINT ( 'NONE',  ( -3.250000000000004441, 5.629165124598849879, 0.000000000000000000 ) ) ;
#2456 = CARTESIAN_POINT ( 'NONE',  ( 228.5935732249376429, 306.3651924111320000, -184.8000000000004945 ) ) ;
#2457 = ORIENTED_EDGE ( 'NONE', *, *, #8828, .F. ) ;
#2458 = ORIENTED_EDGE ( 'NONE', *, *, #4543, .T. ) ;
#2459 = DIRECTION ( 'NONE',  ( -1.000000000000000000, -0.000000000000000000, -0.000000000000000000 ) ) ;
#2460 = ADVANCED_FACE ( 'NONE', ( #7460 ), #5181, .F. ) ;
#2461 = DIRECTION ( 'NONE',  ( -0.000000000000000000, 0.000000000000000000, 1.000000000000000000 ) ) ;
#2462 = CARTESIAN_POINT ( 'NONE',  ( -3.436319922987618902, 2.634841920961291439, -3.531542292955721862 ) ) ;
#2463 = DIRECTION ( 'NONE',  ( 0.000000000000000000, 0.000000000000000000, -1.000000000000000000 ) ) ;
#2464 = DIRECTION ( 'NONE',  ( -1.000000000000000000, 0.000000000000000000, 0.000000000000000000 ) ) ;
#2465 = EDGE_LOOP ( 'NONE', ( #377, #5264, #7707, #6521, #7492, #14525 ) ) ;
#2466 = DIRECTION ( 'NONE',  ( 0.000000000000000000, 0.000000000000000000, -1.000000000000000000 ) ) ;
#2467 = ORIENTED_EDGE ( 'NONE', *, *, #11904, .F. ) ;
#2468 = ORIENTED_EDGE ( 'NONE', *, *, #13088, .F. ) ;
#2469 = LINE ( 'NONE', #155, #8755 ) ;
#2470 = DIRECTION ( 'NONE',  ( 1.000000000000000000, 0.000000000000000000, 0.000000000000000000 ) ) ;
#2471 = CARTESIAN_POINT ( 'NONE',  ( 610.0000000000000000, 10.00000000000005507, -190.0000000000000000 ) ) ;
#2472 = ORIENTED_EDGE ( 'NONE', *, *, #13700, .F. ) ;
#2473 = DIRECTION ( 'NONE',  ( 1.000000000000000000, 0.000000000000000000, 0.000000000000000000 ) ) ;
#2474 = EDGE_CURVE ( 'NONE', #9849, #7201, #587, .T. ) ;
#2475 = FACE_OUTER_BOUND ( 'NONE', #3623, .T. ) ;
#2476 = CARTESIAN_POINT ( 'NONE',  ( 440.1783540539411774, 278.3868002927282532, 210.0000000000000000 ) ) ;
#2477 = DIRECTION ( 'NONE',  ( -0.000000000000000000, -0.000000000000000000, -1.000000000000000000 ) ) ;
#2478 = ORIENTED_EDGE ( 'NONE', *, *, #13536, .F. ) ;
#2479 = DIRECTION ( 'NONE',  ( 1.000000000000000000, 0.000000000000000000, -0.000000000000000000 ) ) ;
#2480 = ORIENTED_EDGE ( 'NONE', *, *, #9254, .F. ) ;
#2481 = ADVANCED_FACE ( 'NONE', ( #1717 ), #6220, .F. ) ;
#2482 = ORIENTED_EDGE ( 'NONE', *, *, #5036, .T. ) ;
#2483 = CARTESIAN_POINT ( 'NONE',  ( 635.0000000000000000, 160.0000000000000284, -225.5000000000000000 ) ) ;
#2484 = DIRECTION ( 'NONE',  ( 1.000000000000000000, 0.000000000000000000, 0.000000000000000000 ) ) ;
#2485 = DIRECTION ( 'NONE',  ( 0.9578262852211524292, -0.2873478855663418874, -0.000000000000000000 ) ) ;
#2486 = ORIENTED_EDGE ( 'NONE', *, *, #7998, .T. ) ;
#2487 = CARTESIAN_POINT ( 'NONE',  ( 459.7035746174796031, 294.6698471414878782, -210.0000000000000000 ) ) ;
#2488 = EDGE_CURVE ( 'NONE', #4304, #4981, #12435, .T. ) ;
#2489 = B_SPLINE_CURVE_WITH_KNOTS ( 'NONE', 3,
 ( #1736, #609, #10590, #14004, #14066, #6090 ),
 .UNSPECIFIED., .F., .F.,
 ( 4, 2, 4 ),
 ( 0.01506847346324403751, 0.01653041426658208995, 0.01799235506992014066 ),
 .UNSPECIFIED. ) ;
#2490 = PLANE ( 'NONE',  #13493 ) ;
#2491 = PLANE ( 'NONE',  #13452 ) ;
#2492 = CARTESIAN_POINT ( 'NONE',  ( 3.453038570460273071, 2.625189405340834448, -3.535263753543585352 ) ) ;
#2493 = ORIENTED_EDGE ( 'NONE', *, *, #12109, .T. ) ;
#2494 = DIRECTION ( 'NONE',  ( 0.000000000000000000, 0.000000000000000000, 1.000000000000000000 ) ) ;
#2495 = CARTESIAN_POINT ( 'NONE',  ( -5.619193549420757883, -4.261310591078458110, -5.875704392893551287 ) ) ;
#2496 = LINE ( 'NONE', #8384, #433 ) ;
#2497 = ORIENTED_EDGE ( 'NONE', *, *, #9135, .F. ) ;
#2498 = EDGE_CURVE ( 'NONE', #12112, #1071, #5144, .T. ) ;
#2499 = CARTESIAN_POINT ( 'NONE',  ( 6.507056549636238252, 2.993353539201077496, 4.999999999999999112 ) ) ;
#2500 = VERTEX_POINT ( 'NONE', #1847 ) ;
#2501 = EDGE_LOOP ( 'NONE', ( #8907, #593, #7904, #13270 ) ) ;
#2502 = DIRECTION ( 'NONE',  ( -1.000000000000000000, 0.000000000000000000, 0.000000000000000000 ) ) ;
#2503 = ADVANCED_FACE ( 'NONE', ( #13010 ), #2739, .F. ) ;
#2504 = CARTESIAN_POINT ( 'NONE',  ( 443.6584422793565636, 264.0194060144110608, 187.0000000000000000 ) ) ;
#2505 = PRODUCT_DEFINITION_SHAPE ( 'NONE', 'NONE',  #5588 ) ;
#2506 = DIRECTION ( 'NONE',  ( 0.000000000000000000, 0.000000000000000000, -1.000000000000000000 ) ) ;
#2507 = CARTESIAN_POINT ( 'NONE',  ( 446.3084422793565409, 264.0194060144110608, -187.0000000000000000 ) ) ;
#2508 = ORIENTED_EDGE ( 'NONE', *, *, #7645, .T. ) ;
#2509 = DIRECTION ( 'NONE',  ( 0.9578262852211514300, -0.2873478855663454401, -0.000000000000000000 ) ) ;
#2510 = DIRECTION ( 'NONE',  ( 0.000000000000000000, 0.000000000000000000, -1.000000000000000000 ) ) ;
#2511 = CARTESIAN_POINT ( 'NONE',  ( 635.0000000000000000, 160.0000000000000284, 208.5000000000000000 ) ) ;
#2512 = LINE ( 'NONE', #1415, #936 ) ;
#2513 = VECTOR ( 'NONE', #11450, 1000.000000000000000 ) ;
#2514 = VERTEX_POINT ( 'NONE', #2903 ) ;
#2515 = ORIENTED_EDGE ( 'NONE', *, *, #3104, .T. ) ;
#2516 = PLANE ( 'NONE',  #6764 ) ;
#2517 = LINE ( 'NONE', #4898, #11078 ) ;
#2518 = PRODUCT_RELATED_PRODUCT_CATEGORY ( 'part', '', ( #13038 ) ) ;
#2519 = CARTESIAN_POINT ( 'NONE',  ( 6.327632967268630004, 3.313549392874629795, 4.260764098153893897 ) ) ;
#2520 = B_SPLINE_CURVE_WITH_KNOTS ( 'NONE', 3,
 ( #6658, #5694, #9015, #6869, #12552 ),
 .UNSPECIFIED., .F., .F.,
 ( 4, 1, 4 ),
 ( 0.000000000000000000, 0.002886751345948132454, 0.005773502691896264909 ),
 .UNSPECIFIED. ) ;
#2522 = ORIENTED_EDGE ( 'NONE', *, *, #5409, .F. ) ;
#2521 = VECTOR ( 'NONE', #5896, 1000.000000000000000 ) ;
#2523 = ADVANCED_FACE ( 'NONE', ( #7401 ), #11888, .T. ) ;
#2524 = AXIS2_PLACEMENT_3D ( 'NONE', #14594, #3384, #7942 ) ;
#2525 = ORIENTED_EDGE ( 'NONE', *, *, #12151, .T. ) ;
#2526 = DIRECTION ( 'NONE',  ( -0.000000000000000000, -0.000000000000000000, 1.000000000000000000 ) ) ;
#2527 = DIRECTION ( 'NONE',  ( -0.000000000000000000, 0.000000000000000000, -1.000000000000000000 ) ) ;
#2528 = ADVANCED_FACE ( 'NONE', ( #13148 ), #1632, .T. ) ;
#2529 = MANIFOLD_SOLID_BREP ( 'Base-Extrude', #14002 ) ;
#2530 = CARTESIAN_POINT ( 'NONE',  ( 6.534224484704354907, 5.901860969583193395, 3.353103961394464287E-14 ) ) ;
#2531 = CARTESIAN_POINT ( 'NONE',  ( 0.000000000000000000, 0.000000000000000000, 190.0000000000000000 ) ) ;
#2532 = DIRECTION ( 'NONE',  ( -1.000000000000000000, 0.000000000000000000, 0.000000000000000000 ) ) ;
#2533 = APPLICATION_CONTEXT ( 'automotive_design' ) ;
#2534 = ORIENTED_EDGE ( 'NONE', *, *, #13069, .T. ) ;
#2535 = LINE ( 'NONE', #11680, #11313 ) ;
#2536 = ORIENTED_EDGE ( 'NONE', *, *, #4940, .F. ) ;
#2537 = ORIENTED_EDGE ( 'NONE', *, *, #58, .T. ) ;
#2538 = AXIS2_PLACEMENT_3D ( 'NONE', #8528, #4920, #9567 ) ;
#2539 = AXIS2_PLACEMENT_3D ( 'NONE', #4039, #4329, #835 ) ;
#2540 = PRODUCT_DEFINITION_SHAPE ( 'NONE', 'NONE',  #14643 ) ;
#2541 = EDGE_CURVE ( 'NONE', #14499, #13769, #11958, .T. ) ;
#2542 = CARTESIAN_POINT ( 'NONE',  ( 637.0568832135862749, 155.4426727739092655, -211.0000000000000000 ) ) ;
#2543 = CARTESIAN_POINT ( 'NONE',  ( 0.000000000000000000, 0.000000000000000000, -4.000000000000000000 ) ) ;
#2544 = VERTEX_POINT ( 'NONE', #4221 ) ;
#2545 = DIRECTION ( 'NONE',  ( -1.000000000000000000, 0.000000000000000000, 0.000000000000000000 ) ) ;
#2546 = CARTESIAN_POINT ( 'NONE',  ( 6.500000000000000888, -4.076778466486154606, -6.121917890101376436 ) ) ;
#2547 = AXIS2_PLACEMENT_3D ( 'NONE', #6636, #12304, #13206 ) ;
#2548 = AXIS2_PLACEMENT_3D ( 'NONE', #9623, #14273, #4103 ) ;
#2549 = AXIS2_PLACEMENT_3D ( 'NONE', #12721, #11396, #1285 ) ;
#2550 = DIRECTION ( 'NONE',  ( 1.000000000000000000, 0.000000000000000000, 0.000000000000000000 ) ) ;
#2551 = PLANE ( 'NONE',  #12307 ) ;
#2552 = VECTOR ( 'NONE', #5814, 1000.000000000000227 ) ;
#2553 = VERTEX_POINT ( 'NONE', #6657 ) ;
#2554 = FACE_OUTER_BOUND ( 'NONE', #10763, .T. ) ;
#2555 = ORIENTED_EDGE ( 'NONE', *, *, #9808, .T. ) ;
#2556 = B_SPLINE_CURVE_WITH_KNOTS ( 'NONE', 3,
 ( #4333, #6613, #13325, #2023, #7717, #8887, #11114, #8606, #7494, #9939, #993, #913, #5356, #3154, #7656, #2996, #1888, #7579, #11991, #14290 ),
 .UNSPECIFIED., .F., .F.,
 ( 4, 2, 2, 2, 2, 2, 2, 2, 2, 4 ),
 ( 5.551115123125782702E-17, 0.001037574205614438111, 0.002075148411228820711, 0.003112722616843203310, 0.003631509719650373360, 0.004150296822457543409, 0.005187871028071766415, 0.006225445233685987685, 0.007263019439300210690, 0.008300593644914432828 ),
 .UNSPECIFIED. ) ;
#2557 = MANIFOLD_SOLID_BREP ( 'AdvancedHole1', #11148 ) ;
#2558 = ORIENTED_EDGE ( 'NONE', *, *, #2136, .F. ) ;
#2559 = CARTESIAN_POINT ( 'NONE',  ( 590.0000000000000000, 10.00000000000005507, 210.0000000000000000 ) ) ;
#2560 = EDGE_CURVE ( 'NONE', #3448, #1307, #5845, .T. ) ;
#2561 = VECTOR ( 'NONE', #11667, 1000.000000000000000 ) ;
#2562 = VECTOR ( 'NONE', #7394, 1000.000000000000227 ) ;
#2563 = DIRECTION ( 'NONE',  ( -0.9578262852211515410, 0.2873478855663446074, -0.000000000000000000 ) ) ;
#2564 = CARTESIAN_POINT ( 'NONE',  ( 3.098410542199072637, -7.060458129626440815, -1.000000000000000000 ) ) ;
#2565 = VERTEX_POINT ( 'NONE', #10997 ) ;
#2566 = CARTESIAN_POINT ( 'NONE',  ( 0.000000000000000000, -4.330127018922194537, -2.500000000000000444 ) ) ;
#2567 = AXIS2_PLACEMENT_3D ( 'NONE', #4312, #9774, #8513 ) ;
#2568 = DIRECTION ( 'NONE',  ( 0.000000000000000000, 0.000000000000000000, 1.000000000000000000 ) ) ;
#2569 = FACE_OUTER_BOUND ( 'NONE', #9843, .T. ) ;
#2570 = PLANE ( 'NONE',  #3114 ) ;
#2571 = ORIENTED_EDGE ( 'NONE', *, *, #8909, .F. ) ;
#2572 = CONICAL_SURFACE ( 'NONE', #1403, 3.309499999999999886, 0.7853981633974407295 ) ;
#2573 = AXIS2_PLACEMENT_3D ( 'NONE', #13352, #3464, #12457 ) ;
#2574 = CARTESIAN_POINT ( 'NONE',  ( 5.991014884144049368, -4.330127018922198978, -2.500000000000000444 ) ) ;
#2575 = DIRECTION ( 'NONE',  ( 0.000000000000000000, 1.000000000000000000, 0.000000000000000000 ) ) ;
#2576 = EDGE_LOOP ( 'NONE', ( #5534, #12423, #9463, #524 ) ) ;
#2577 = CARTESIAN_POINT ( 'NONE',  ( 6.242789945155967857, 0.9948955795114693412, 5.105232858000414708 ) ) ;
#2578 = ORIENTED_EDGE ( 'NONE', *, *, #11158, .F. ) ;
#2579 = ORIENTED_EDGE ( 'NONE', *, *, #2767, .T. ) ;
#2580 = CARTESIAN_POINT ( 'NONE',  ( -0.9108756637653833144, 6.979659189792688956, -6.219623095965475024 ) ) ;
#2581 = EDGE_CURVE ( 'NONE', #5903, #264, #13224, .T. ) ;
#2582 = VECTOR ( 'NONE', #12371, 1000.000000000000000 ) ;
#2583 = CARTESIAN_POINT ( 'NONE',  ( 639.0000000000000000, 156.0000000000000000, -233.5000000000000000 ) ) ;
#2584 = ADVANCED_FACE ( 'NONE', ( #6509 ), #11218, .F. ) ;
#2585 = AXIS2_PLACEMENT_3D ( 'NONE', #2423, #4865, #3453 ) ;
#2586 = AXIS2_PLACEMENT_3D ( 'NONE', #14163, #4057, #5307 ) ;
#2587 = MANIFOLD_SOLID_BREP ( '<sliding track>-<M5 Clearance Hole1>', #13758 ) ;
#2588 = ADVANCED_FACE ( 'NONE', ( #13581 ), #7905, .F. ) ;
#2589 = LINE ( 'NONE', #3410, #5681 ) ;
#2590 = EDGE_CURVE ( 'NONE', #442, #12943, #11031, .T. ) ;
#2591 = AXIS2_PLACEMENT_3D ( 'NONE', #1045, #5843, #138 ) ;
#2592 = CARTESIAN_POINT ( 'NONE',  ( 0.000000000000000000, 0.000000000000000000, 0.000000000000000000 ) ) ;
#2593 = VERTEX_POINT ( 'NONE', #9305 ) ;
#2594 = AXIS2_PLACEMENT_3D ( 'NONE', #11900, #8660, #3136 ) ;
#2595 = EDGE_CURVE ( 'NONE', #5365, #6317, #8435, .T. ) ;
#2596 = FACE_OUTER_BOUND ( 'NONE', #11255, .T. ) ;
#2597 = CARTESIAN_POINT ( 'NONE',  ( 470.8287951810180516, 310.9528939902474463, -210.0000000000000000 ) ) ;
#2598 = DIRECTION ( 'NONE',  ( 0.000000000000000000, 0.000000000000000000, 1.000000000000000000 ) ) ;
#2599 = VECTOR ( 'NONE', #7198, 1000.000000000000114 ) ;
#2600 = CARTESIAN_POINT ( 'NONE',  ( 6.534224484704352243, 2.950930484791584263, 5.111161529262904679 ) ) ;
#2601 = AXIS2_PLACEMENT_3D ( 'NONE', #1284, #3427, #10285 ) ;
#2602 = ORIENTED_EDGE ( 'NONE', *, *, #430, .T. ) ;
#2603 = EDGE_LOOP ( 'NONE', ( #2074, #12432 ) ) ;
#2604 = CARTESIAN_POINT ( 'NONE',  ( 6.818286579240217193, -1.325012739682874141, -6.208253321455268647 ) ) ;
#2605 = CARTESIAN_POINT ( 'NONE',  ( 723.8855453127955570, 217.2873478855649694, -177.6000000000007901 ) ) ;
#2606 = DIRECTION ( 'NONE',  ( -0.9578262852210943645, 0.2873478855665353993, 0.000000000000000000 ) ) ;
#2607 = VECTOR ( 'NONE', #8502, 1000.000000000000114 ) ;
#2608 = VECTOR ( 'NONE', #1714, 1000.000000000000227 ) ;
#2609 = EDGE_CURVE ( 'NONE', #3145, #2790, #3185, .T. ) ;
#2610 = CIRCLE ( 'NONE', #5916, 0.2500000000000002220 ) ;
#2611 = ORIENTED_EDGE ( 'NONE', *, *, #123, .T. ) ;
#2612 = EDGE_CURVE ( 'NONE', #13279, #11011, #1400, .T. ) ;
#2613 = AXIS2_PLACEMENT_3D ( 'NONE', #11424, #3458, #2266 ) ;
#2614 = CARTESIAN_POINT ( 'NONE',  ( 164.3243839102495656, 402.9042173714779551, -190.0000000000000000 ) ) ;
#2615 = CARTESIAN_POINT ( 'NONE',  ( -1.149515148933662080E-15, -4.736529461166056443, -3.681130640444383317 ) ) ;
#2616 = DIRECTION ( 'NONE',  ( 0.9578262852211508749, -0.2873478855663467724, 0.000000000000000000 ) ) ;
#2617 = MANIFOLD_SOLID_BREP ( 'M5 Clearance Hole1', #11159 ) ;
#2618 = DIRECTION ( 'NONE',  ( 0.000000000000000000, 1.000000000000000000, -1.287488025362403787E-15 ) ) ;
#2619 = CARTESIAN_POINT ( 'NONE',  ( 2.999999999999999112, 3.464101615137752166, 2.000000000000003553 ) ) ;
#2620 = CYLINDRICAL_SURFACE ( 'NONE', #897, 2.199999999999701306 ) ;
#2621 = AXIS2_PLACEMENT_3D ( 'NONE', #4525, #4597, #3477 ) ;
#2622 = VERTEX_POINT ( 'NONE', #4882 ) ;
#2623 = AXIS2_PLACEMENT_3D ( 'NONE', #5030, #6040, #12767 ) ;
#2624 = CARTESIAN_POINT ( 'NONE',  ( 5.441945782601302462, 4.363644636964922441, -0.3576316571898402463 ) ) ;
#2625 = ORIENTED_EDGE ( 'NONE', *, *, #6511, .T. ) ;
#2626 = ORIENTED_EDGE ( 'NONE', *, *, #4337, .F. ) ;
#2627 = DIRECTION ( 'NONE',  ( -1.000000000000000000, 0.000000000000000000, 0.000000000000000000 ) ) ;
#2628 = VECTOR ( 'NONE', #8665, 1000.000000000000000 ) ;
#2629 = EDGE_CURVE ( 'NONE', #4733, #2291, #2662, .T. ) ;
#2630 = DIRECTION ( 'NONE',  ( 1.000000000000000000, 0.000000000000000000, 0.000000000000000000 ) ) ;
#2631 = CIRCLE ( 'NONE', #12512, 4.199999999999981526 ) ;
#2632 = VECTOR ( 'NONE', #7245, 1000.000000000000000 ) ;
#2633 = LINE ( 'NONE', #6014, #14313 ) ;
#2634 = FACE_OUTER_BOUND ( 'NONE', #5663, .T. ) ;
#2635 = VERTEX_POINT ( 'NONE', #12619 ) ;
#2636 = CARTESIAN_POINT ( 'NONE',  ( 0.6920835326022565237, 4.454600218803884459, -3.597382984111579862 ) ) ;
#2637 = CARTESIAN_POINT ( 'NONE',  ( 6.815964470354069604, -1.383691465878164717, -6.173460172893482145 ) ) ;
#2638 = CARTESIAN_POINT ( 'NONE',  ( -3.453038570459499024, -2.625189405340453419, -3.535263753545272891 ) ) ;
#2639 = FILL_AREA_STYLE ('',( #4040 ) ) ;
#2640 = SURFACE_SIDE_STYLE ('',( #6100 ) ) ;
#2641 = EDGE_LOOP ( 'NONE', ( #6484, #1215, #9398, #4878 ) ) ;
#2642 = CARTESIAN_POINT ( 'NONE',  ( -3.761337442881754015E-15, 3.838309248099015747, 3.351853367131007122 ) ) ;
#2643 = ORIENTED_EDGE ( 'NONE', *, *, #12581, .F. ) ;
#2644 = CIRCLE ( 'NONE', #12059, 5.000000000000000000 ) ;
#2645 = MANIFOLD_SOLID_BREP ( 'HeadFillet', #7861 ) ;
#2646 = DIRECTION ( 'NONE',  ( -1.000000000000000000, 0.000000000000000000, 0.000000000000000000 ) ) ;
#2647 = LINE ( 'NONE', #12668, #11303 ) ;
#2648 = CARTESIAN_POINT ( 'NONE',  ( 2.000000000000000444, 3.464101615137754830, -3.142992957459231018 ) ) ;
#2649 = ORIENTED_EDGE ( 'NONE', *, *, #622, .F. ) ;
#2650 = PLANE ( 'NONE',  #6633 ) ;
#2651 = CARTESIAN_POINT ( 'NONE',  ( 642.0000000000000000, 153.0000000000000284, -225.5000000000000000 ) ) ;
#2652 = CARTESIAN_POINT ( 'NONE',  ( -9.999999999999957367, 376.8992337277236970, -190.0000000000000000 ) ) ;
#2653 = CARTESIAN_POINT ( 'NONE',  ( 0.5449313310647804220, 4.304185902836899835, -3.316620875263383894 ) ) ;
#2654 = EDGE_CURVE ( 'NONE', #11133, #488, #3162, .T. ) ;
#2655 = ORIENTED_EDGE ( 'NONE', *, *, #10016, .F. ) ;
#2656 = EDGE_LOOP ( 'NONE', ( #724, #9745, #8062, #171, #7414, #5546, #2244, #3375 ) ) ;
#2657 = CARTESIAN_POINT ( 'NONE',  ( 6.271006797790669829, -0.9853839345309193254, -5.106080050406711202 ) ) ;
#2658 = ORIENTED_EDGE ( 'NONE', *, *, #10835, .T. ) ;
#2659 = CARTESIAN_POINT ( 'NONE',  ( 6.204449577088272605, 0.9975080636026212311, 5.000000000000000000 ) ) ;
#2660 = VERTEX_POINT ( 'NONE', #2725 ) ;
#2661 = ORIENTED_EDGE ( 'NONE', *, *, #1966, .F. ) ;
#2662 = LINE ( 'NONE', #56, #6794 ) ;
#2663 = DIRECTION ( 'NONE',  ( 1.000000000000000000, 0.000000000000000000, 0.000000000000000000 ) ) ;
#2664 = DIRECTION ( 'NONE',  ( -1.000000000000000000, -0.000000000000000000, -0.000000000000000000 ) ) ;
#2665 = LINE ( 'NONE', #6881, #11080 ) ;
#2666 = DIRECTION ( 'NONE',  ( 0.000000000000000000, 0.000000000000000000, 1.000000000000000000 ) ) ;
#2667 = UNCERTAINTY_MEASURE_WITH_UNIT (LENGTH_MEASURE( 1.000000000000000082E-05 ), #14207, 'distance_accuracy_value', 'NONE');
#2668 = AXIS2_PLACEMENT_3D ( 'NONE', #14504, #3072, #14444 ) ;
#2669 = DIRECTION ( 'NONE',  ( 0.000000000000000000, 0.000000000000000000, -1.000000000000000000 ) ) ;
#2670 = EDGE_CURVE ( 'NONE', #734, #5903, #14102, .T. ) ;
#2671 = VERTEX_POINT ( 'NONE', #13959 ) ;
#2672 = CARTESIAN_POINT ( 'NONE',  ( 497.0347780250717733, -149.1104334075207589, 189.9999999999986358 ) ) ;
#2673 = CARTESIAN_POINT ( 'NONE',  ( 610.8620436566991430, 188.5525593289319488, -184.8000000000000398 ) ) ;
#2674 = DIRECTION ( 'NONE',  ( 1.000000000000000000, 0.000000000000000000, 0.000000000000000000 ) ) ;
#2675 = EDGE_CURVE ( 'NONE', #1319, #9797, #3986, .T. ) ;
#2676 = CARTESIAN_POINT ( 'NONE',  ( 6.518095160332174842, 2.933089652807376435, 5.080260301816937663 ) ) ;
#2677 = EDGE_LOOP ( 'NONE', ( #12262, #12023 ) ) ;
#2678 = ORIENTED_EDGE ( 'NONE', *, *, #5120, .T. ) ;
#2679 = CARTESIAN_POINT ( 'NONE',  ( 144.7991633467111683, 386.6211705227183870, -210.0000000000000000 ) ) ;
#2680 = DIRECTION ( 'NONE',  ( 0.000000000000000000, 0.000000000000000000, 1.000000000000000000 ) ) ;
#2681 = ADVANCED_FACE ( 'NONE', ( #7519 ), #9671, .F. ) ;
#2682 = DIRECTION ( 'NONE',  ( -0.000000000000000000, 0.000000000000000000, -1.000000000000000000 ) ) ;
#2683 = ADVANCED_FACE ( 'NONE', ( #574 ), #12843, .F. ) ;
#2684 = FACE_OUTER_BOUND ( 'NONE', #1826, .T. ) ;
#2685 = EDGE_LOOP ( 'NONE', ( #13978, #10029, #13818, #1557, #12283 ) ) ;
#2686 = FACE_OUTER_BOUND ( 'NONE', #8957, .T. ) ;
#2687 = CARTESIAN_POINT ( 'NONE',  ( 6.481779955677546390, -2.910222513313224457, -5.040653254389286353 ) ) ;
#2688 = DIRECTION ( 'NONE',  ( -1.000000000000000000, 0.000000000000000000, -0.000000000000000000 ) ) ;
#2689 = CARTESIAN_POINT ( 'NONE',  ( 641.0000000000000000, 166.0000000000000284, -187.5000000000000000 ) ) ;
#2690 = PLANE ( 'NONE',  #9377 ) ;
#2691 = EDGE_LOOP ( 'NONE', ( #13364, #12574, #13404, #8767 ) ) ;
#2692 = FACE_OUTER_BOUND ( 'NONE', #10073, .T. ) ;
#2693 = ORIENTED_EDGE ( 'NONE', *, *, #3278, .F. ) ;
#2694 = VERTEX_POINT ( 'NONE', #8561 ) ;
#2695 = CARTESIAN_POINT ( 'NONE',  ( -4.000000000000000000, 0.7924765000094600165, -0.05906175389889745803 ) ) ;
#2696 = EDGE_CURVE ( 'NONE', #611, #11996, #1838, .T. ) ;
#2697 = EDGE_CURVE ( 'NONE', #9095, #4166, #11499, .T. ) ;
#2698 = DIRECTION ( 'NONE',  ( 1.000000000000000000, 0.000000000000000000, 0.000000000000000000 ) ) ;
#2699 = DIRECTION ( 'NONE',  ( 1.000000000000000000, 0.000000000000000000, 0.000000000000000000 ) ) ;
#2700 = CARTESIAN_POINT ( 'NONE',  ( 640.0000000000000000, 160.0000000000000284, -211.0000000000000000 ) ) ;
#2701 = VERTEX_POINT ( 'NONE', #11931 ) ;
#2702 = FACE_OUTER_BOUND ( 'NONE', #2691, .T. ) ;
#2703 = CARTESIAN_POINT ( 'NONE',  ( -10.00000000000000000, 371.6790804732683569, 187.0000000000000000 ) ) ;
#2704 = CARTESIAN_POINT ( 'NONE',  ( 6.445127866599364985, -3.194847394660945916, 4.687657648742338701 ) ) ;
#2705 =( LENGTH_UNIT ( ) NAMED_UNIT ( * ) SI_UNIT ( .MILLI., .METRE. ) );
#2706 = ORIENTED_EDGE ( 'NONE', *, *, #11506, .T. ) ;
#2707 = CARTESIAN_POINT ( 'NONE',  ( 1.600000000000000089, 0.000000000000000000, 0.000000000000000000 ) ) ;
#2708 = EDGE_LOOP ( 'NONE', ( #12529, #3000, #13955, #4120 ) ) ;
#2709 = DIRECTION ( 'NONE',  ( -0.9578262852211517631, 0.2873478855663438858, -0.000000000000000000 ) ) ;
#2710 = CARTESIAN_POINT ( 'NONE',  ( 0.000000000000000000, 0.000000000000000000, 0.000000000000000000 ) ) ;
#2711 = DIRECTION ( 'NONE',  ( 0.000000000000000000, 0.000000000000000000, 1.000000000000000000 ) ) ;
#2712 = ORIENTED_EDGE ( 'NONE', *, *, #186, .F. ) ;
#2713 = LINE ( 'NONE', #14081, #6409 ) ;
#2714 = CARTESIAN_POINT ( 'NONE',  ( -2.682243648011671588, -3.070208061305317759, -0.04852650426602272971 ) ) ;
#2715 = CARTESIAN_POINT ( 'NONE',  ( 6.500000000000000888, 2.536640449112275153, -0.3753468889000217690 ) ) ;
#2716 = FACE_OUTER_BOUND ( 'NONE', #2939, .T. ) ;
#2717 = ORIENTED_EDGE ( 'NONE', *, *, #12846, .T. ) ;
#2718 = EDGE_CURVE ( 'NONE', #13064, #12163, #13068, .T. ) ;
#2719 = FILL_AREA_STYLE ('',( #6122 ) ) ;
#2720 = CARTESIAN_POINT ( 'NONE',  ( 631.0000000000000000, 155.9999999999999432, -233.5000000000000000 ) ) ;
#2721 = VERTEX_POINT ( 'NONE', #8479 ) ;
#2722 = DIRECTION ( 'NONE',  ( 1.000000000000000000, 0.000000000000000000, 0.000000000000000000 ) ) ;
#2723 = EDGE_LOOP ( 'NONE', ( #11965, #3945, #5282, #12334 ) ) ;
#2724 = EDGE_LOOP ( 'NONE', ( #12186, #5469, #2534, #13215 ) ) ;
#2725 = CARTESIAN_POINT ( 'NONE',  ( 152.8304684875957662, 364.5911659626319761, -190.0000000000000000 ) ) ;
#2726 = DIRECTION ( 'NONE',  ( -0.9578262852211525402, 0.2873478855663419429, 0.000000000000000000 ) ) ;
#2727 = ADVANCED_FACE ( 'NONE', ( #6341 ), #12991, .T. ) ;
#2728 = FACE_OUTER_BOUND ( 'NONE', #2451, .T. ) ;
#2729 = ADVANCED_FACE ( 'NONE', ( #2883 ), #5033, .T. ) ;
#2730 = DIRECTION ( 'NONE',  ( 0.000000000000000000, 0.000000000000000000, 1.000000000000000000 ) ) ;
#2731 = DIRECTION ( 'NONE',  ( -0.000000000000000000, -0.000000000000000000, -1.000000000000000000 ) ) ;
#2732 = VERTEX_POINT ( 'NONE', #8400 ) ;
#2733 = CARTESIAN_POINT ( 'NONE',  ( -9.999999999999998224, 376.8992337277234128, -187.0000000000000000 ) ) ;
#2734 = LINE ( 'NONE', #11726, #9172 ) ;
#2735 = DIRECTION ( 'NONE',  ( 0.000000000000000000, 0.000000000000000000, 1.000000000000000000 ) ) ;
#2736 = CARTESIAN_POINT ( 'NONE',  ( 6.500000000000000000, 3.752776749732573247, -0.8000000000000003775 ) ) ;
#2737 = ORIENTED_EDGE ( 'NONE', *, *, #3249, .F. ) ;
#2738 = ORIENTED_EDGE ( 'NONE', *, *, #507, .T. ) ;
#2739 = PLANE ( 'NONE',  #9855 ) ;
#2740 = CARTESIAN_POINT ( 'NONE',  ( 641.0000000000000000, 154.0000000000000568, -187.5000000000000000 ) ) ;
#2741 = CARTESIAN_POINT ( 'NONE',  ( -4.639619758716985842, 4.826867782832376719, -0.1499059597315285375 ) ) ;
#2742 = EDGE_CURVE ( 'NONE', #12153, #8153, #4069, .T. ) ;
#2743 = DIRECTION ( 'NONE',  ( 0.000000000000000000, 0.5000000000000009992, 0.8660254037844380415 ) ) ;
#2744 = ORIENTED_EDGE ( 'NONE', *, *, #2027, .F. ) ;
#2745 = DIRECTION ( 'NONE',  ( -0.2873478855663480491, -0.9578262852211507639, 0.000000000000000000 ) ) ;
#2746 = CARTESIAN_POINT ( 'NONE',  ( 6.534224484704354907, -2.950930484791607800, -5.111161529262896686 ) ) ;
#2747 = DIRECTION ( 'NONE',  ( -0.000000000000000000, -0.000000000000000000, 1.000000000000000000 ) ) ;
#2748 = EDGE_CURVE ( 'NONE', #3179, #9848, #7299, .T. ) ;
#2749 = CARTESIAN_POINT ( 'NONE',  ( 164.3243839102495656, 402.9042173714779551, -210.0000000000000000 ) ) ;
#2750 = DIRECTION ( 'NONE',  ( 0.000000000000000000, -0.4999999999999989453, 0.8660254037844391517 ) ) ;
#2751 = CARTESIAN_POINT ( 'NONE',  ( 0.3572655899081558228, -2.309401076758485161, 3.999999999999999112 ) ) ;
#2752 = PRESENTATION_STYLE_ASSIGNMENT (( #4775 ) ) ;
#2753 = PRODUCT_DEFINITION_SHAPE ( 'NONE', 'NONE',  #14618 ) ;
#2754 = ORIENTED_EDGE ( 'NONE', *, *, #2150, .F. ) ;
#2755 = CARTESIAN_POINT ( 'NONE',  ( 0.5469614295415388128, -4.303013824935362663, -3.535263753543555598 ) ) ;
#2756 = ORIENTED_EDGE ( 'NONE', *, *, #10128, .T. ) ;
#2757 = ORIENTED_EDGE ( 'NONE', *, *, #1525, .T. ) ;
#2758 = CARTESIAN_POINT ( 'NONE',  ( -4.000000000000000000, 0.000000000000000000, 0.000000000000000000 ) ) ;
#2759 = EDGE_CURVE ( 'NONE', #214, #503, #7739, .T. ) ;
#2760 = VECTOR ( 'NONE', #7455, 1000.000000000000000 ) ;
#2761 = FACE_BOUND ( 'NONE', #10258, .T. ) ;
#2762 = VECTOR ( 'NONE', #12787, 1000.000000000000000 ) ;
#2763 = DIRECTION ( 'NONE',  ( 0.000000000000000000, 0.000000000000000000, -1.000000000000000000 ) ) ;
#2764 = CARTESIAN_POINT ( 'NONE',  ( -4.000000000000000000, -2.309401076758515803, -0.4999999999999995559 ) ) ;
#2765 = AXIS2_PLACEMENT_3D ( 'NONE', #3412, #3562, #9157 ) ;
#2766 = VERTEX_POINT ( 'NONE', #5249 ) ;
#2767 = EDGE_CURVE ( 'NONE', #9543, #11816, #14246, .T. ) ;
#2768 = CARTESIAN_POINT ( 'NONE',  ( 144.7991633467111399, 386.6211705227183870, 210.0000000000000000 ) ) ;
#2769 = DIRECTION ( 'NONE',  ( -0.000000000000000000, 0.000000000000000000, -1.000000000000000000 ) ) ;
#2770 = EDGE_CURVE ( 'NONE', #12569, #10525, #6494, .T. ) ;
#2771 = CARTESIAN_POINT ( 'NONE',  ( 6.355827204229362870, -5.411702751981846582, 0.8440485055075603871 ) ) ;
#2772 = FACE_BOUND ( 'NONE', #10036, .T. ) ;
#2773 = SHAPE_REPRESENTATION_RELATIONSHIP ( 'NONE' , 'NONE' ,  #9980, #6513 ) ;
#2774 = ORIENTED_EDGE ( 'NONE', *, *, #349, .T. ) ;
#2775 = EDGE_CURVE ( 'NONE', #525, #739, #4281, .T. ) ;
#2776 = FILL_AREA_STYLE_COLOUR ( '', #5422 ) ;
#2777 = CARTESIAN_POINT ( 'NONE',  ( 6.506987859255528583, 2.925375531177293986, -5.066899051217878203 ) ) ;
#2778 = CIRCLE ( 'NONE', #7251, 8.105212085995399107 ) ;
#2779 = ORIENTED_EDGE ( 'NONE', *, *, #10399, .F. ) ;
#2780 = DIRECTION ( 'NONE',  ( 0.000000000000000000, 0.000000000000000000, 1.000000000000000000 ) ) ;
#2781 = CARTESIAN_POINT ( 'NONE',  ( 639.0000000000000000, 164.0000000000000000, -233.5000000000000000 ) ) ;
#2782 = CYLINDRICAL_SURFACE ( 'NONE', #3577, 4.199999999999981526 ) ;
#2783 = VECTOR ( 'NONE', #989, 1000.000000000000114 ) ;
#2784 = EDGE_LOOP ( 'NONE', ( #4869, #11981, #9283, #7174 ) ) ;
#2785 = CARTESIAN_POINT ( 'NONE',  ( 609.9277849535120595, 190.4148309465319358, 190.0300000000000296 ) ) ;
#2786 = EDGE_CURVE ( 'NONE', #6408, #4046, #2077, .T. ) ;
#2787 = DIRECTION ( 'NONE',  ( -0.000000000000000000, -0.000000000000000000, -1.000000000000000000 ) ) ;
#2788 = DIRECTION ( 'NONE',  ( -0.000000000000000000, -0.000000000000000000, -1.000000000000000000 ) ) ;
#2789 = CARTESIAN_POINT ( 'NONE',  ( 3.540020015735602765, 2.810662092924382627, -3.602146406945867962 ) ) ;
#2790 = VERTEX_POINT ( 'NONE', #4199 ) ;
#2791 = CARTESIAN_POINT ( 'NONE',  ( 0.2500000000000002220, 0.000000000000000000, 0.000000000000000000 ) ) ;
#2792 = LINE ( 'NONE', #4948, #2284 ) ;
#2793 = ORIENTED_EDGE ( 'NONE', *, *, #9284, .T. ) ;
#2794 = ORIENTED_EDGE ( 'NONE', *, *, #357, .T. ) ;
#2795 = CIRCLE ( 'NONE', #11039, 4.799999999999968736 ) ;
#2796 = AXIS2_PLACEMENT_3D ( 'NONE', #9839, #4020, #3053 ) ;
#2797 = VERTEX_POINT ( 'NONE', #7738 ) ;
#2798 = CARTESIAN_POINT ( 'NONE',  ( -20.63749999999999574, 8.541911424052788811E-16, 6.975000000000000533 ) ) ;
#2799 = ADVANCED_FACE ( 'NONE', ( #934 ), #2115, .T. ) ;
#2800 = CARTESIAN_POINT ( 'NONE',  ( 229.2257385731834063, 308.4724102386176128, -177.6000000000002217 ) ) ;
#2801 = VECTOR ( 'NONE', #5063, 1000.000000000000000 ) ;
#2802 = CARTESIAN_POINT ( 'NONE',  ( 655.0000000000000000, 160.0000000000000284, 187.5000000000000000 ) ) ;
#2803 = EDGE_CURVE ( 'NONE', #2876, #5286, #8686, .T. ) ;
#2804 = DIRECTION ( 'NONE',  ( 0.000000000000000000, 0.000000000000000000, -1.000000000000000000 ) ) ;
#2805 = AXIS2_PLACEMENT_3D ( 'NONE', #1279, #7859, #7780 ) ;
#2806 = AXIS2_PLACEMENT_3D ( 'NONE', #1771, #3997, #654 ) ;
#2807 = UNCERTAINTY_MEASURE_WITH_UNIT (LENGTH_MEASURE( 1.000000000000000082E-05 ), #555, 'distance_accuracy_value', 'NONE');
#2808 = CARTESIAN_POINT ( 'NONE',  ( 707.5067158355133188, 162.6912496279604738, 177.6000000000001648 ) ) ;
#2809 = ORIENTED_EDGE ( 'NONE', *, *, #9732, .F. ) ;
#2810 = FACE_OUTER_BOUND ( 'NONE', #2784, .T. ) ;
#2811 = CARTESIAN_POINT ( 'NONE',  ( 8.500000000000000000, 2.886751345948122882, -5.000000000000000000 ) ) ;
#2812 = DIRECTION ( 'NONE',  ( 0.000000000000000000, 0.000000000000000000, -1.000000000000000000 ) ) ;
#2813 = CIRCLE ( 'NONE', #5647, 2.199999999999984635 ) ;
#2814 = FACE_OUTER_BOUND ( 'NONE', #11072, .T. ) ;
#2815 = EDGE_LOOP ( 'NONE', ( #274, #13787, #14344, #12061 ) ) ;
#2816 = VERTEX_POINT ( 'NONE', #8845 ) ;
#2817 = CARTESIAN_POINT ( 'NONE',  ( -9.511508594537124495, 378.5275384125996538, 187.0000000000000284 ) ) ;
#2818 = DIRECTION ( 'NONE',  ( -1.000000000000000000, -0.000000000000000000, -0.000000000000000000 ) ) ;
#2819 = CIRCLE ( 'NONE', #7293, 4.000000000000000000 ) ;
#2820 = DIRECTION ( 'NONE',  ( -0.5000000000000006661, -0.8660254037844382635, 0.000000000000000000 ) ) ;
#2821 = APPLICATION_CONTEXT ( 'automotive_design' ) ;
#2822 = SHAPE_REPRESENTATION ( 'MAS-180', ( #4786, #3356, #11588, #5247, #10897, #13486, #7122, #8066, #2408, #1706, #12541, #5717, #9730, #1946, #9958, #3364, #5018, #6430, #35, #7131, #11603, #3602, #8543, #11834, #759, #10908, #4302, #1228, #2892, #4075, #11132 ), #10430 ) ;
#2823 = DIRECTION ( 'NONE',  ( -1.000000000000000000, 0.000000000000000000, 0.000000000000000000 ) ) ;
#2824 = ORIENTED_EDGE ( 'NONE', *, *, #2864, .F. ) ;
#2825 = CARTESIAN_POINT ( 'NONE',  ( 10.00000000000000000, 386.5596934910894902, -210.0000000000000000 ) ) ;
#2826 = CARTESIAN_POINT ( 'NONE',  ( 4.000000000000000000, 0.7924765000094659007, -0.05906175389889852662 ) ) ;
#2827 = LINE ( 'NONE', #13427, #5208 ) ;
#2828 = AXIS2_PLACEMENT_3D ( 'NONE', #14234, #4122, #8611 ) ;
#2829 = CIRCLE ( 'NONE', #1879, 2.041999999999999815 ) ;
#2830 = CARTESIAN_POINT ( 'NONE',  ( 0.000000000000000000, 0.000000000000000000, 0.000000000000000000 ) ) ;
#2831 = CARTESIAN_POINT ( 'NONE',  ( 1.600000000000000089, 0.000000000000000000, 2.700000000000000178 ) ) ;
#2832 = DIRECTION ( 'NONE',  ( -0.000000000000000000, -0.000000000000000000, -1.000000000000000000 ) ) ;
#2833 = EDGE_CURVE ( 'NONE', #6946, #8674, #3743, .T. ) ;
#2834 = ORIENTED_EDGE ( 'NONE', *, *, #11620, .T. ) ;
#2835 = CARTESIAN_POINT ( 'NONE',  ( 2.807080416178989513, -3.225969019225150003, -3.502507215260505014 ) ) ;
#2836 = EDGE_LOOP ( 'NONE', ( #8114, #3156, #8120, #2014 ) ) ;
#2837 = VERTEX_POINT ( 'NONE', #12092 ) ;
#2838 = AXIS2_PLACEMENT_3D ( 'NONE', #9373, #9306, #2502 ) ;
#2839 = DIRECTION ( 'NONE',  ( -0.9578262852211513190, 0.2873478855663453846, 0.000000000000000000 ) ) ;
#2840 = AXIS2_PLACEMENT_3D ( 'NONE', #7240, #9247, #1629 ) ;
#2841 = CIRCLE ( 'NONE', #12977, 3.999999999999999112 ) ;
#2842 = AXIS2_PLACEMENT_3D ( 'NONE', #3398, #7894, #44 ) ;
#2843 = PLANE ( 'NONE',  #8956 ) ;
#2844 = DIRECTION ( 'NONE',  ( 0.9578262852211525402, -0.2873478855663419429, -0.000000000000000000 ) ) ;
#2845 = FACE_OUTER_BOUND ( 'NONE', #13127, .T. ) ;
#2846 = CIRCLE ( 'NONE', #4507, 7.399999999999999467 ) ;
#2847 = VERTEX_POINT ( 'NONE', #11053 ) ;
#2848 = CARTESIAN_POINT ( 'NONE',  ( 3.861362476283255685, 2.629030857715988656, -3.671615880910370500 ) ) ;
#2849 = DIRECTION ( 'NONE',  ( 1.387778780781446464E-15, -2.775557561562892929E-15, 1.000000000000000000 ) ) ;
#2850 = CIRCLE ( 'NONE', #8504, 0.7499999999999997780 ) ;
#2851 = CARTESIAN_POINT ( 'NONE',  ( -2.756197834950067094, -3.027510591568735254, -3.223146290109809797 ) ) ;
#2852 = CYLINDRICAL_SURFACE ( 'NONE', #766, 2.200000000000007283 ) ;
#2853 = SURFACE_STYLE_FILL_AREA ( #8232 ) ;
#2854 = EDGE_CURVE ( 'NONE', #5286, #2876, #10335, .T. ) ;
#2855 = VERTEX_POINT ( 'NONE', #14308 ) ;
#2856 = CIRCLE ( 'NONE', #13220, 5.249999999999976907 ) ;
#2857 = PRESENTATION_LAYER_ASSIGNMENT (  '', '', ( #3565 ) ) ;
#2858 = DIRECTION ( 'NONE',  ( 0.000000000000000000, -1.000000000000000000, 0.000000000000000000 ) ) ;
#2859 = CONTEXT_DEPENDENT_SHAPE_REPRESENTATION ( #10553, #625 ) ;
#2860 = VERTEX_POINT ( 'NONE', #4494 ) ;
#2861 = ADVANCED_FACE ( 'NONE', ( #9810 ), #14526, .T. ) ;
#2863 = PLANE ( 'NONE',  #5628 ) ;
#2862 = AXIS2_PLACEMENT_3D ( 'NONE', #13566, #3536, #6927 ) ;
#2864 = EDGE_CURVE ( 'NONE', #12665, #352, #3098, .T. ) ;
#2865 = LINE ( 'NONE', #3837, #14610 ) ;
#2867 = DIRECTION ( 'NONE',  ( 0.000000000000000000, 0.000000000000000000, -1.000000000000000000 ) ) ;
#2866 = CIRCLE ( 'NONE', #5689, 4.199999999999981526 ) ;
#2868 = ADVANCED_FACE ( 'NONE', ( #14385 ), #3390, .F. ) ;
#2869 =( GEOMETRIC_REPRESENTATION_CONTEXT ( 3 ) GLOBAL_UNCERTAINTY_ASSIGNED_CONTEXT ( ( #8266 ) ) GLOBAL_UNIT_ASSIGNED_CONTEXT ( ( #13389, #5787, #10289 ) ) REPRESENTATION_CONTEXT ( 'NONE', 'WORKASPACE' ) );
#2870 = VERTEX_POINT ( 'NONE', #6425 ) ;
#2871 = DIRECTION ( 'NONE',  ( -0.000000000000000000, 0.000000000000000000, -1.000000000000000000 ) ) ;
#2872 = FACE_OUTER_BOUND ( 'NONE', #3651, .T. ) ;
#2873 = DIRECTION ( 'NONE',  ( 1.000000000000000000, 0.000000000000000000, 0.000000000000000000 ) ) ;
#2874 = CIRCLE ( 'NONE', #13482, 7.399999999999999467 ) ;
#2875 = LINE ( 'NONE', #6744, #12921 ) ;
#2876 = VERTEX_POINT ( 'NONE', #8782 ) ;
#2877 = CARTESIAN_POINT ( 'NONE',  ( 6.371919382990606451, -1.972754410575520367, -5.108792907957607099 ) ) ;
#2878 = DIRECTION ( 'NONE',  ( -1.000000000000000000, -0.000000000000000000, -0.000000000000000000 ) ) ;
#2879 = ORIENTED_EDGE ( 'NONE', *, *, #1835, .T. ) ;
#2880 = VERTEX_POINT ( 'NONE', #6706 ) ;
#2881 = MECHANICAL_DESIGN_GEOMETRIC_PRESENTATION_REPRESENTATION (  '', ( #9948 ), #14196 ) ;
#2882 = ORIENTED_EDGE ( 'NONE', *, *, #13158, .F. ) ;
#2883 = FACE_OUTER_BOUND ( 'NONE', #2138, .T. ) ;
#2884 = ADVANCED_FACE ( 'NONE', ( #14603 ), #10924, .T. ) ;
#2885 = ADVANCED_FACE ( 'NONE', ( #8995 ), #4516, .F. ) ;
#2886 = DIRECTION ( 'NONE',  ( -0.000000000000000000, -0.000000000000000000, -1.000000000000000000 ) ) ;
#2887 = CIRCLE ( 'NONE', #29, 7.000000000000000000 ) ;
#2888 = CARTESIAN_POINT ( 'NONE',  ( -10.00000000000000000, 0.000000000000000000, 210.0000000000000000 ) ) ;
#2889 = EDGE_CURVE ( 'NONE', #6611, #10150, #13788, .T. ) ;
#2890 = PRODUCT_DEFINITION_SHAPE ( 'NONE', 'NONE',  #13442 ) ;
#2891 = LINE ( 'NONE', #14181, #6391 ) ;
#2892 = AXIS2_PLACEMENT_3D ( 'NONE', #805, #8638, #2812 ) ;
#2893 = CYLINDRICAL_SURFACE ( 'NONE', #9310, 2.649999999999985700 ) ;
#2894 = ORIENTED_EDGE ( 'NONE', *, *, #14304, .T. ) ;
#2895 = CARTESIAN_POINT ( 'NONE',  ( 0.000000000000000000, 4.330127018922191873, 2.500000000000005773 ) ) ;
#2896 = DIRECTION ( 'NONE',  ( -1.000000000000000000, 0.000000000000000000, 0.000000000000000000 ) ) ;
#2897 = DIRECTION ( 'NONE',  ( -1.000000000000000000, 0.000000000000000000, 0.000000000000000000 ) ) ;
#2898=STYLED_ITEM('',(#14653),#11938);
#2900 = VECTOR ( 'NONE', #3639, 1000.000000000000000 ) ;
#2899 = DIRECTION ( 'NONE',  ( -0.2873478855663454401, -0.9578262852211514300, 0.000000000000000000 ) ) ;
#2901 = EDGE_LOOP ( 'NONE', ( #8125, #3345 ) ) ;
#2902 = VERTEX_POINT ( 'NONE', #11482 ) ;
#2903 = CARTESIAN_POINT ( 'NONE',  ( -2.595115354961444076, -7.673029147243174641, -1.000000000000000000 ) ) ;
#2904 = CARTESIAN_POINT ( 'NONE',  ( 0.000000000000000000, 0.000000000000000000, -4.974599999999998801 ) ) ;
#2905 = PRODUCT ( 'roller', 'roller', '', ( #8858 ) ) ;
#2906 = CARTESIAN_POINT ( 'NONE',  ( -10.00000000000045297, 371.6790804732678453, 1.178702027242996938E-12 ) ) ;
#2907 = PRESENTATION_LAYER_ASSIGNMENT (  '', '', ( #1004 ) ) ;
#2908 = DIRECTION ( 'NONE',  ( 1.000000000000000000, 0.000000000000000000, -0.000000000000000000 ) ) ;
#2909 = ORIENTED_EDGE ( 'NONE', *, *, #10247, .F. ) ;
#2910 = CARTESIAN_POINT ( 'NONE',  ( -1.400000000000000133, 6.245698675651501825E-16, 5.100000000000000533 ) ) ;
#2911 = CARTESIAN_POINT ( 'NONE',  ( 5.589124336233334489, 4.278671059407959554, -6.219623095966918314 ) ) ;
#2912 = DIRECTION ( 'NONE',  ( 0.000000000000000000, -0.000000000000000000, 1.000000000000000000 ) ) ;
#2913 = CARTESIAN_POINT ( 'NONE',  ( 627.2408731339806991, 284.9098836221797342, 190.0000000000001990 ) ) ;
#2914 = PLANE ( 'NONE',  #1150 ) ;
#2915 = CARTESIAN_POINT ( 'NONE',  ( 637.5000000000000000, 160.0000000000000284, -217.5000000000000284 ) ) ;
#2916 = ORIENTED_EDGE ( 'NONE', *, *, #13451, .T. ) ;
#2917 = PLANE ( 'NONE',  #8480 ) ;
#2918 = EDGE_LOOP ( 'NONE', ( #3461, #2602, #9198, #5501, #6203, #10799 ) ) ;
#2919 = ORIENTED_EDGE ( 'NONE', *, *, #5293, .F. ) ;
#2920 = LINE ( 'NONE', #6235, #1198 ) ;
#2921 = DIRECTION ( 'NONE',  ( 1.000000000000000000, 0.000000000000000000, -0.000000000000000000 ) ) ;
#2922 = EDGE_CURVE ( 'NONE', #1995, #13316, #175, .T. ) ;
#2923 = CARTESIAN_POINT ( 'NONE',  ( 631.0000000000000000, 164.0000000000000284, -233.5000000000000000 ) ) ;
#2924 = DIRECTION ( 'NONE',  ( 1.000000000000000000, 0.000000000000000000, 0.000000000000000000 ) ) ;
#2925 = EDGE_CURVE ( 'NONE', #11833, #9079, #2795, .T. ) ;
#2926 = ORIENTED_EDGE ( 'NONE', *, *, #10772, .T. ) ;
#2927 = CARTESIAN_POINT ( 'NONE',  ( 3.399999999999999911, 0.000000000000000000, -7.554475477074173106 ) ) ;
#2928 = CARTESIAN_POINT ( 'NONE',  ( 642.3047950750125210, 161.9631091326946830, 210.0000120000000265 ) ) ;
#2929 = CARTESIAN_POINT ( 'NONE',  ( -122.9652219749301736, 36.88956659247854475, 189.9999999999986358 ) ) ;
#2930 = DIRECTION ( 'NONE',  ( 0.000000000000000000, 0.000000000000000000, -1.000000000000000000 ) ) ;
#2931 = SURFACE_STYLE_FILL_AREA ( #12136 ) ;
#2932 = ORIENTED_EDGE ( 'NONE', *, *, #4778, .T. ) ;
#2933 = DIRECTION ( 'NONE',  ( 0.000000000000000000, 0.000000000000000000, -1.000000000000000000 ) ) ;
#2934 = CARTESIAN_POINT ( 'NONE',  ( 6.534533895392293346, 2.951347675328718001, -5.111884124469663782 ) ) ;
#2935 = ORIENTED_EDGE ( 'NONE', *, *, #1079, .T. ) ;
#2936 = CARTESIAN_POINT ( 'NONE',  ( 6.837824896291514243, 3.947820044545427454, -6.564402953523716278 ) ) ;
#2937 = ADVANCED_FACE ( 'NONE', ( #9212, #12600 ), #10466, .F. ) ;
#2938 = CARTESIAN_POINT ( 'NONE',  ( 610.0000000000000000, 175.0000000000000568, 210.0000000000000000 ) ) ;
#2939 = EDGE_LOOP ( 'NONE', ( #3305, #923 ) ) ;
#2940 = DIRECTION ( 'NONE',  ( 0.000000000000000000, -0.000000000000000000, -1.000000000000000000 ) ) ;
#2941 = DIRECTION ( 'NONE',  ( 1.000000000000000000, 0.000000000000000000, 0.000000000000000000 ) ) ;
#2942 = CARTESIAN_POINT ( 'NONE',  ( 227.7315295682386136, 303.4917135554685501, -184.8000000000004945 ) ) ;
#2943 =( NAMED_UNIT ( * ) SI_UNIT ( $, .STERADIAN. ) SOLID_ANGLE_UNIT ( ) );
#2944 = EDGE_LOOP ( 'NONE', ( #1572, #13039 ) ) ;
#2945 = ADVANCED_FACE ( 'NONE', ( #4864, #4573 ), #13854, .T. ) ;
#2946 = CARTESIAN_POINT ( 'NONE',  ( 6.244297270355322560, -0.4917101305082268725, -5.105276777067913052 ) ) ;
#2947 = SURFACE_STYLE_USAGE ( .BOTH. , #10761 ) ;
#2948 = B_SPLINE_CURVE_WITH_KNOTS ( 'NONE', 3,
 ( #3705, #6137, #10555, #12777 ),
 .UNSPECIFIED., .F., .F.,
 ( 4, 4 ),
 ( 2.380735200832039115E-07, 0.002921158011986728538 ),
 .UNSPECIFIED. ) ;
#2949 = VERTEX_POINT ( 'NONE', #3451 ) ;
#2950 = VERTEX_POINT ( 'NONE', #2258 ) ;
#2951 = DIRECTION ( 'NONE',  ( 1.000000000000000000, 0.000000000000000000, 0.000000000000000000 ) ) ;
#2952 = DIRECTION ( 'NONE',  ( 0.000000000000000000, 0.000000000000000000, 1.000000000000000000 ) ) ;
#2953 = EDGE_CURVE ( 'NONE', #2565, #13081, #9395, .T. ) ;
#2954 = CARTESIAN_POINT ( 'NONE',  ( 642.5000000000001137, 160.0000000000000284, -210.0000059999999849 ) ) ;
#2955 = CARTESIAN_POINT ( 'NONE',  ( -4.154094228333820915, -2.398367420967594921, -3.721909803043257803 ) ) ;
#2956 = PRODUCT_DEFINITION_CONTEXT ( 'detailed design', #2821, 'design' ) ;
#2957 = CARTESIAN_POINT ( 'NONE',  ( 708.1388811837593948, 164.7984674554458309, -179.7999999999999261 ) ) ;
#2958 = VERTEX_POINT ( 'NONE', #11271 ) ;
#2959 = ADVANCED_FACE ( 'NONE', ( #2422 ), #10174, .T. ) ;
#2960 = DIRECTION ( 'NONE',  ( -0.2873478855663454401, -0.9578262852211513190, 0.000000000000000000 ) ) ;
#2961 = DIRECTION ( 'NONE',  ( 0.2873478855663434972, 0.9578262852211520961, 0.000000000000000000 ) ) ;
#2963 = EDGE_CURVE ( 'NONE', #7913, #9391, #3751, .T. ) ;
#2962 = LINE ( 'NONE', #4218, #14159 ) ;
#2964 = ORIENTED_EDGE ( 'NONE', *, *, #6483, .T. ) ;
#2965 = PRODUCT_RELATED_PRODUCT_CATEGORY ( 'part', '', ( #13474 ) ) ;
#2966 = ORIENTED_EDGE ( 'NONE', *, *, #1697, .F. ) ;
#2967 = CARTESIAN_POINT ( 'NONE',  ( 0.1481481481481481122, -4.797713218419819903, 0.000000000000000000 ) ) ;
#2968 = CARTESIAN_POINT ( 'NONE',  ( -6.500000000000000000, -3.752776749732573247, -0.8000000000000003775 ) ) ;
#2969 = CARTESIAN_POINT ( 'NONE',  ( 609.7493509738548028, 188.4639666770506494, -189.3135794259398494 ) ) ;
#2970 = CARTESIAN_POINT ( 'NONE',  ( 33.50000000000000000, 2.789133085058097101E-16, -2.054999999999999716 ) ) ;
#2971 = ORIENTED_EDGE ( 'NONE', *, *, #3175, .F. ) ;
#2972 = LINE ( 'NONE', #9832, #5262 ) ;
#2973 = CARTESIAN_POINT ( 'NONE',  ( 470.8287951810180516, 310.9528939902474463, -210.0000000000000000 ) ) ;
#2974 = DIRECTION ( 'NONE',  ( -1.000000000000000000, -0.000000000000000000, -0.000000000000000000 ) ) ;
#2975 = ORIENTED_EDGE ( 'NONE', *, *, #1065, .F. ) ;
#2976 = CARTESIAN_POINT ( 'NONE',  ( -2.100000000000000089, 2.571758278209441957E-16, -4.694516984716113228 ) ) ;
#2977 = CARTESIAN_POINT ( 'NONE',  ( 455.5035746174796714, 294.6698471414878782, 190.0000000000000568 ) ) ;
#2978 = DIRECTION ( 'NONE',  ( 1.102263794768336594E-15, 3.674212649225140308E-15, 1.000000000000000000 ) ) ;
#2979 =( NAMED_UNIT ( * ) PLANE_ANGLE_UNIT ( ) SI_UNIT ( $, .RADIAN. ) );
#2980 = ORIENTED_EDGE ( 'NONE', *, *, #10462, .T. ) ;
#2982 = CYLINDRICAL_SURFACE ( 'NONE', #12965, 7.500000000000000000 ) ;
#2981 = PRODUCT_RELATED_PRODUCT_CATEGORY ( 'part', '', ( #11936 ) ) ;
#2983 = ORIENTED_EDGE ( 'NONE', *, *, #10270, .T. ) ;
#2984 = ORIENTED_EDGE ( 'NONE', *, *, #3700, .T. ) ;
#2985 = LINE ( 'NONE', #9991, #9709 ) ;
#2986 = EDGE_CURVE ( 'NONE', #10129, #4375, #11351, .T. ) ;
#2987 = DIRECTION ( 'NONE',  ( 0.000000000000000000, -1.224646799147353454E-16, 1.000000000000000000 ) ) ;
#2988 = EDGE_CURVE ( 'NONE', #9517, #8693, #12207, .T. ) ;
#2989 = VERTEX_POINT ( 'NONE', #258 ) ;
#2990 = VERTEX_POINT ( 'NONE', #8159 ) ;
#2991 = CARTESIAN_POINT ( 'NONE',  ( 0.000000000000000000, 0.000000000000000000, 6.250000000000000000 ) ) ;
#2992 = CARTESIAN_POINT ( 'NONE',  ( 638.7771423527817660, 166.5533979126570614, 210.0000120000000265 ) ) ;
#2993 = DIRECTION ( 'NONE',  ( -0.000000000000000000, -0.000000000000000000, -1.000000000000000000 ) ) ;
#2994 = DIRECTION ( 'NONE',  ( 0.000000000000000000, 0.000000000000000000, 1.000000000000000000 ) ) ;
#2995 = ORIENTED_EDGE ( 'NONE', *, *, #8081, .T. ) ;
#2996 = CARTESIAN_POINT ( 'NONE',  ( 609.7645211877446627, 186.0291131959509698, 186.4810828243464016 ) ) ;
#2997 = CARTESIAN_POINT ( 'NONE',  ( -9.511508594537124495, 378.5275384125996538, -187.0000000000000284 ) ) ;
#2998 = CONTEXT_DEPENDENT_SHAPE_REPRESENTATION ( #12063, #7953 ) ;
#2999 =( BOUNDED_SURFACE ( )  B_SPLINE_SURFACE ( 3, 2, ( 
 ( #6258, #2236, #13386 ),
 ( #10756, #3282, #11026 ),
 ( #5158, #7651, #908 ),
 ( #6684, #11179, #5564 ),
 ( #4462, #2462, #10142 ),
 ( #4617, #9104, #4773 ) ),
 .UNSPECIFIED., .F., .F., .T. ) 
 B_SPLINE_SURFACE_WITH_KNOTS ( ( 4, 2, 4 ),
 ( 3, 3 ),
 ( 0.02032853247518125531, 0.02278863295364820865, 0.02524873343211516200 ),
 ( 0.000000000000000000, 1.000000000000000000 ),
 .UNSPECIFIED. ) 
 GEOMETRIC_REPRESENTATION_ITEM ( )  RATIONAL_B_SPLINE_SURFACE ( (
 ( 1.000000000000000000, 0.8047781615896836271, 1.000000000000000000),
 ( 1.000000000000000000, 0.8123767586289967202, 1.000000000000000000),
 ( 1.000000000000000000, 0.8190662415563443322, 1.000000000000000000),
 ( 1.000000000000000000, 0.8192361015669982205, 1.000000000000000000),
 ( 1.000000000000000000, 0.8126135807103181952, 1.000000000000000000),
 ( 1.000000000000000000, 0.8047712338318587788, 1.000000000000000000) ) ) 
 REPRESENTATION_ITEM ( '' )  SURFACE ( )  );
#3000 = ORIENTED_EDGE ( 'NONE', *, *, #5185, .T. ) ;
#3001 = CARTESIAN_POINT ( 'NONE',  ( -8.542937654374687995, 0.000000000000000000, -6.800000000000000711 ) ) ;
#3002 = EDGE_CURVE ( 'NONE', #10447, #9874, #8027, .T. ) ;
#3003 = ORIENTED_EDGE ( 'NONE', *, *, #2697, .T. ) ;
#3004 = VECTOR ( 'NONE', #12514, 1000.000000000000227 ) ;
#3005 = CARTESIAN_POINT ( 'NONE',  ( 6.815830331203685866, 0.6619522098568483282, -6.171384342982615401 ) ) ;
#3006 = DIRECTION ( 'NONE',  ( -0.2873478855663470499, -0.9578262852211508749, 0.000000000000000000 ) ) ;
#3007 = ORIENTED_EDGE ( 'NONE', *, *, #2021, .F. ) ;
#3008 = CARTESIAN_POINT ( 'NONE',  ( 112.9652219749295341, 376.5507399164317803, 190.0000000000000000 ) ) ;
#3009 = PLANE ( 'NONE',  #1405 ) ;
#3010 =( GEOMETRIC_REPRESENTATION_CONTEXT ( 3 ) GLOBAL_UNCERTAINTY_ASSIGNED_CONTEXT ( ( #7693 ) ) GLOBAL_UNIT_ASSIGNED_CONTEXT ( ( #8397, #13801, #13954 ) ) REPRESENTATION_CONTEXT ( 'NONE', 'WORKASPACE' ) );
#3011 = VECTOR ( 'NONE', #7034, 1000.000000000000000 ) ;
#3012 = CARTESIAN_POINT ( 'NONE',  ( -8.074769166705396017, 378.0965165842501392, -187.0000000000000284 ) ) ;
#3013 = SURFACE_STYLE_USAGE ( .BOTH. , #13122 ) ;
#3014 = VERTEX_POINT ( 'NONE', #9288 ) ;
#3015 = CIRCLE ( 'NONE', #11480, 2.649999999999985700 ) ;
#3016 = CARTESIAN_POINT ( 'NONE',  ( 6.244004651191001010, 4.663678638742294602, 2.132808149174402867 ) ) ;
#3017 = VERTEX_POINT ( 'NONE', #2559 ) ;
#3018 = APPLICATION_CONTEXT ( 'automotive_design' ) ;
#3019 = ADVANCED_FACE ( 'NONE', ( #3532 ), #7061, .T. ) ;
#3020 = ORIENTED_EDGE ( 'NONE', *, *, #5314, .T. ) ;
#3021 = CARTESIAN_POINT ( 'NONE',  ( 139.8040310085880833, 355.9707293956415697, -190.0000000000000000 ) ) ;
#3022 = AXIS2_PLACEMENT_3D ( 'NONE', #9689, #8577, #9608 ) ;
#3024 = VECTOR ( 'NONE', #12983, 1000.000000000000000 ) ;
#3023 = CYLINDRICAL_SURFACE ( 'NONE', #8224, 5.199999999999732836 ) ;
#3025 = DIRECTION ( 'NONE',  ( 0.9578262852211513190, -0.2873478855663455511, 1.110223024625158513E-15 ) ) ;
#3026 = CARTESIAN_POINT ( 'NONE',  ( 7.240873133980807452, 470.9098836221798479, -190.0000000000001990 ) ) ;
#3027 = CARTESIAN_POINT ( 'NONE',  ( 0.000000000000000000, 0.000000000000000000, -7.554475477074173106 ) ) ;
#3028 = EDGE_LOOP ( 'NONE', ( #5579, #7466, #3469, #11581 ) ) ;
#3029 = AXIS2_PLACEMENT_3D ( 'NONE', #5882, #13719, #12667 ) ;
#3030 = VECTOR ( 'NONE', #5918, 1000.000000000000000 ) ;
#3031 = AXIS2_PLACEMENT_3D ( 'NONE', #3787, #3708, #7309 ) ;
#3032 = CARTESIAN_POINT ( 'NONE',  ( 459.7035746174795463, 294.6698471414878782, 210.0000000000000000 ) ) ;
#3033 = CARTESIAN_POINT ( 'NONE',  ( 0.000000000000000000, 0.000000000000000000, -1.000000000000000000 ) ) ;
#3034 = SHAPE_DEFINITION_REPRESENTATION ( #14411, #9337 ) ;
#3035 = ADVANCED_FACE ( 'NONE', ( #11563, #8540, #12971 ), #9923, .T. ) ;
#3036 = LINE ( 'NONE', #3183, #1895 ) ;
#3037 = VERTEX_POINT ( 'NONE', #3835 ) ;
#3038 = ORIENTED_EDGE ( 'NONE', *, *, #10054, .T. ) ;
#3039 = CARTESIAN_POINT ( 'NONE',  ( -20.63749999999999929, 0.000000000000000000, 0.000000000000000000 ) ) ;
#3040 = CARTESIAN_POINT ( 'NONE',  ( 2.999999999999999112, 2.309401076758500704, -4.000000000000000000 ) ) ;
#3041 = ADVANCED_FACE ( 'NONE', ( #6186, #562, #5148, #3904, #8386, #4322 ), #2863, .F. ) ;
#3042 = CARTESIAN_POINT ( 'NONE',  ( 609.8848581100098727, 185.7487647174620520, -185.4822770966949008 ) ) ;
#3043 = CONICAL_SURFACE ( 'NONE', #1388, 2.499999999999946709, 1.029744259999984646 ) ;
#3044 = ADVANCED_FACE ( 'NONE', ( #7360 ), #4933, .T. ) ;
#3045 = CIRCLE ( 'NONE', #10351, 5.000000000000004441 ) ;
#3046 = DIRECTION ( 'NONE',  ( -0.000000000000000000, 0.000000000000000000, -1.000000000000000000 ) ) ;
#3047 = VERTEX_POINT ( 'NONE', #5083 ) ;
#3048 = EDGE_CURVE ( 'NONE', #6453, #3563, #7393, .T. ) ;
#3049 = LINE ( 'NONE', #1855, #9272 ) ;
#3050 = ORIENTED_EDGE ( 'NONE', *, *, #6990, .F. ) ;
#3051 = DIRECTION ( 'NONE',  ( -1.000000000000000000, -0.000000000000000000, -0.000000000000000000 ) ) ;
#3052 = DIRECTION ( 'NONE',  ( -0.2873478855663441633, -0.9578262852211516520, 0.000000000000000000 ) ) ;
#3053 = DIRECTION ( 'NONE',  ( 0.9578262852211513190, -0.2873478855663453846, 0.000000000000000000 ) ) ;
#3054 = ORIENTED_EDGE ( 'NONE', *, *, #11417, .T. ) ;
#3055 = AXIS2_PLACEMENT_3D ( 'NONE', #10999, #2279, #11295 ) ;
#3056 = DIRECTION ( 'NONE',  ( 0.000000000000000000, 0.000000000000000000, -1.000000000000000000 ) ) ;
#3057 = VECTOR ( 'NONE', #5520, 1000.000000000000000 ) ;
#3058 = ORIENTED_EDGE ( 'NONE', *, *, #7142, .F. ) ;
#3059 = EDGE_LOOP ( 'NONE', ( #11049, #12357, #12708, #11338 ) ) ;
#3060 = CARTESIAN_POINT ( 'NONE',  ( 640.0000000000000000, 160.0000000000000284, -210.0000000000000000 ) ) ;
#3061 = ADVANCED_FACE ( 'NONE', ( #8316 ), #3991, .T. ) ;
#3062 = EDGE_CURVE ( 'NONE', #13769, #14499, #2087, .T. ) ;
#3063 = CARTESIAN_POINT ( 'NONE',  ( 630.5661054975340676, 158.1613647612965110, -210.0000000000000000 ) ) ;
#3064 = AXIS2_PLACEMENT_3D ( 'NONE', #10610, #9656, #7214 ) ;
#3065 = VERTEX_POINT ( 'NONE', #1747 ) ;
#3066 = EDGE_CURVE ( 'NONE', #1307, #11290, #1594, .T. ) ;
#3067 = VECTOR ( 'NONE', #11534, 1000.000000000000000 ) ;
#3068 = EDGE_LOOP ( 'NONE', ( #13416, #5705, #5230, #9123 ) ) ;
#3069 = CARTESIAN_POINT ( 'NONE',  ( 0.000000000000000000, 0.000000000000000000, 0.000000000000000000 ) ) ;
#3070 = LINE ( 'NONE', #13256, #8958 ) ;
#3071 = CARTESIAN_POINT ( 'NONE',  ( 446.3084422793565409, 264.0194060144110608, -210.0000000000000000 ) ) ;
#3072 = DIRECTION ( 'NONE',  ( 0.000000000000000000, 0.000000000000000000, 1.000000000000000000 ) ) ;
#3073 = AXIS2_PLACEMENT_3D ( 'NONE', #5283, #13167, #9712 ) ;
#3074 = ORIENTED_EDGE ( 'NONE', *, *, #9191, .T. ) ;
#3075 = DIRECTION ( 'NONE',  ( -1.000000000000000000, 0.000000000000000000, 0.000000000000000000 ) ) ;
#3076 = ORIENTED_EDGE ( 'NONE', *, *, #5920, .F. ) ;
#3077 = DIRECTION ( 'NONE',  ( -0.000000000000000000, -1.000000000000000000, -0.000000000000000000 ) ) ;
#3078 = AXIS2_PLACEMENT_3D ( 'NONE', #4098, #8426, #753 ) ;
#3079 = ORIENTED_EDGE ( 'NONE', *, *, #297, .T. ) ;
#3080 = CARTESIAN_POINT ( 'NONE',  ( 10.00000000000000000, 10.00000000000000178, 190.0000000000000000 ) ) ;
#3081 = CIRCLE ( 'NONE', #13212, 2.649999999999985700 ) ;
#3082 = CIRCLE ( 'NONE', #5671, 0.7500000000000000000 ) ;
#3083 = DIRECTION ( 'NONE',  ( 0.000000000000000000, 0.000000000000000000, 1.000000000000000000 ) ) ;
#3084 = ORIENTED_EDGE ( 'NONE', *, *, #281, .T. ) ;
#3085 = LINE ( 'NONE', #3008, #13703 ) ;
#3086 = FACE_BOUND ( 'NONE', #2901, .T. ) ;
#3087 = VECTOR ( 'NONE', #4355, 1000.000000000000000 ) ;
#3088 = STYLED_ITEM ( 'NONE', ( #1904 ), #12520 ) ;
#3089 = PLANE ( 'NONE',  #10432 ) ;
#3090 = SHAPE_REPRESENTATION_RELATIONSHIP ( 'NONE' , 'NONE' ,  #1873, #3907 ) ;
#3091 = ORIENTED_EDGE ( 'NONE', *, *, #3679, .T. ) ;
#3092 = CARTESIAN_POINT ( 'NONE',  ( 5.000000000000000888, 0.000000000000000000, 0.000000000000000000 ) ) ;
#3093 = CARTESIAN_POINT ( 'NONE',  ( -6.500000000000000000, 3.752776749732564809, -0.7999999999999969358 ) ) ;
#3094 = ORIENTED_EDGE ( 'NONE', *, *, #7350, .T. ) ;
#3095 = CIRCLE ( 'NONE', #1250, 4.000000000000000000 ) ;
#3096 = VECTOR ( 'NONE', #4846, 1000.000000000000000 ) ;
#3097 = ORIENTED_EDGE ( 'NONE', *, *, #14584, .T. ) ;
#3098 = LINE ( 'NONE', #7889, #176 ) ;
#3099 = CIRCLE ( 'NONE', #11341, 4.199999999999981526 ) ;
#3100 = PRESENTATION_LAYER_ASSIGNMENT (  '', '', ( #8283 ) ) ;
#3101 = DIRECTION ( 'NONE',  ( 0.000000000000000000, -1.000000000000000000, 3.264827003555233190E-15 ) ) ;
#3102 = CARTESIAN_POINT ( 'NONE',  ( 642.3094156464453590, 161.9516943256562911, -210.0000000000000284 ) ) ;
#3103 = CIRCLE ( 'NONE', #14408, 7.399999999999999467 ) ;
#3104 = EDGE_CURVE ( 'NONE', #13316, #8002, #899, .T. ) ;
#3105 = DIRECTION ( 'NONE',  ( -0.000000000000000000, -0.000000000000000000, 1.000000000000000000 ) ) ;
#3106 = CIRCLE ( 'NONE', #7104, 2.649999999999985700 ) ;
#3107 = PRODUCT_DEFINITION_CONTEXT ( 'detailed design', #7544, 'design' ) ;
#3108 = CARTESIAN_POINT ( 'NONE',  ( 4.078421086530217288, -3.990950201428958621, -1.000000000000000000 ) ) ;
#3109 = ORIENTED_EDGE ( 'NONE', *, *, #2045, .F. ) ;
#3110 =( GEOMETRIC_REPRESENTATION_CONTEXT ( 3 ) GLOBAL_UNCERTAINTY_ASSIGNED_CONTEXT ( ( #12849 ) ) GLOBAL_UNIT_ASSIGNED_CONTEXT ( ( #12118, #2979, #7477 ) ) REPRESENTATION_CONTEXT ( 'NONE', 'WORKASPACE' ) );
#3111 = DIRECTION ( 'NONE',  ( 0.000000000000000000, 0.000000000000000000, -1.000000000000000000 ) ) ;
#3112 = LINE ( 'NONE', #9681, #6582 ) ;
#3113 = CARTESIAN_POINT ( 'NONE',  ( 148.9991633467111569, 386.6211705227183870, -178.5000000000000568 ) ) ;
#3114 = AXIS2_PLACEMENT_3D ( 'NONE', #7220, #6119, #502 ) ;
#3115 = DIRECTION ( 'NONE',  ( -0.000000000000000000, -0.000000000000000000, -1.000000000000000000 ) ) ;
#3116 = ORIENTED_EDGE ( 'NONE', *, *, #8157, .T. ) ;
#3117 = ORIENTED_EDGE ( 'NONE', *, *, #13879, .T. ) ;
#3118 = CIRCLE ( 'NONE', #4532, 4.000000000000000000 ) ;
#3119 = DIRECTION ( 'NONE',  ( 0.000000000000000000, -0.5000000000000018874, -0.8660254037844375974 ) ) ;
#3120 = LINE ( 'NONE', #5398, #9676 ) ;
#3121 = CARTESIAN_POINT ( 'NONE',  ( 609.7152679600854981, 186.3148376777868975, -187.1062553063055418 ) ) ;
#3122 = PRODUCT_DEFINITION_FORMATION_WITH_SPECIFIED_SOURCE ( 'ANY', '', #12531, .NOT_KNOWN. ) ;
#3123 = EDGE_CURVE ( 'NONE', #10957, #2949, #11985, .T. ) ;
#3124 = DIRECTION ( 'NONE',  ( -2.449021377849607626E-15, -3.265361837132810036E-15, 1.000000000000000000 ) ) ;
#3125 = VERTEX_POINT ( 'NONE', #14156 ) ;
#3126 = AXIS2_PLACEMENT_3D ( 'NONE', #7668, #2034, #5308 ) ;
#3127 = CARTESIAN_POINT ( 'NONE',  ( 0.5000000000000000000, -6.429618962271402616, 0.000000000000000000 ) ) ;
#3128 = ORIENTED_EDGE ( 'NONE', *, *, #12605, .F. ) ;
#3129 = ADVANCED_FACE ( 'NONE', ( #2011 ), #10526, .F. ) ;
#3130 = DIRECTION ( 'NONE',  ( 0.000000000000000000, 0.000000000000000000, 1.000000000000000000 ) ) ;
#3131 = DIRECTION ( 'NONE',  ( -0.000000000000000000, -0.000000000000000000, 1.000000000000000000 ) ) ;
#3132 = DIRECTION ( 'NONE',  ( 0.000000000000000000, 0.000000000000000000, 1.000000000000000000 ) ) ;
#3133 = SURFACE_SIDE_STYLE ('',( #6377 ) ) ;
#3134 = ORIENTED_EDGE ( 'NONE', *, *, #6198, .T. ) ;
#3135 = EDGE_CURVE ( 'NONE', #11363, #14011, #11774, .T. ) ;
#3136 = DIRECTION ( 'NONE',  ( 0.000000000000000000, 0.000000000000000000, 1.000000000000000000 ) ) ;
#3137 = VERTEX_POINT ( 'NONE', #7213 ) ;
#3138 = ORIENTED_EDGE ( 'NONE', *, *, #13421, .F. ) ;
#3139 = CARTESIAN_POINT ( 'NONE',  ( -8.505790995054914205, 376.6597771564183859, 187.0000000000000284 ) ) ;
#3140 = CARTESIAN_POINT ( 'NONE',  ( 164.3243839102495656, 402.9042173714779551, -210.0000000000000000 ) ) ;
#3141 = VECTOR ( 'NONE', #615, 1000.000000000000000 ) ;
#3142 = AXIS2_PLACEMENT_3D ( 'NONE', #6667, #12255, #11160 ) ;
#3143 = DIRECTION ( 'NONE',  ( -0.000000000000000000, -0.000000000000000000, -1.000000000000000000 ) ) ;
#3144 = ORIENTED_EDGE ( 'NONE', *, *, #2045, .T. ) ;
#3145 = VERTEX_POINT ( 'NONE', #4049 ) ;
#3146 = CARTESIAN_POINT ( 'NONE',  ( 6.212068001623118008, -5.350125758160992007, 0.7333103599822092811 ) ) ;
#3147 = FACE_OUTER_BOUND ( 'NONE', #13031, .T. ) ;
#3148 = DIRECTION ( 'NONE',  ( 0.2873478855663439413, 0.9578262852211518741, -0.000000000000000000 ) ) ;
#3149 = FACE_OUTER_BOUND ( 'NONE', #6673, .T. ) ;
#3150 = DIRECTION ( 'NONE',  ( 1.000000000000000000, 0.000000000000000000, 0.000000000000000000 ) ) ;
#3151 = COLOUR_RGB ( '',1.000000000000000000, 0.9490196078431372140, 0.9098039215686274384 ) ;
#3152 = VERTEX_POINT ( 'NONE', #3140 ) ;
#3153 = EDGE_CURVE ( 'NONE', #3214, #9710, #12894, .T. ) ;
#3154 = CARTESIAN_POINT ( 'NONE',  ( 609.6994022290995190, 186.4862707338506311, 187.4054488658613593 ) ) ;
#3155 = ITEM_DEFINED_TRANSFORMATION ( 'NONE', 'NONE', #759,  #9440 ) ;
#3156 = ORIENTED_EDGE ( 'NONE', *, *, #3873, .F. ) ;
#3157 = DIRECTION ( 'NONE',  ( -0.000000000000000000, -0.000000000000000000, 1.000000000000000000 ) ) ;
#3158 = EDGE_CURVE ( 'NONE', #8163, #7561, #1851, .T. ) ;
#3159 = VERTEX_POINT ( 'NONE', #10052 ) ;
#3160 = LINE ( 'NONE', #9946, #8237 ) ;
#3161 = CARTESIAN_POINT ( 'NONE',  ( -9.232659125071873696E-16, -0.4883827417527039638, 4.999999999999999112 ) ) ;
#3162 = B_SPLINE_CURVE_WITH_KNOTS ( 'NONE', 3,
 ( #3471, #1759, #5098, #3916, #8333, #8627 ),
 .UNSPECIFIED., .F., .F.,
 ( 4, 2, 4 ),
 ( 8.673617379884035472E-19, 0.0003352299596267569490, 0.0006704599192535130306 ),
 .UNSPECIFIED. ) ;
#3163 = VERTEX_POINT ( 'NONE', #6738 ) ;
#3164 = DIRECTION ( 'NONE',  ( -0.2873478855663454401, -0.9578262852211513190, -4.930380657631323784E-32 ) ) ;
#3165 = CARTESIAN_POINT ( 'NONE',  ( 33.50000000000000000, 2.516649172247810568E-16, -2.054999999999999716 ) ) ;
#3166 = DIRECTION ( 'NONE',  ( 0.000000000000000000, 0.000000000000000000, 1.000000000000000000 ) ) ;
#3167 =( NAMED_UNIT ( * ) PLANE_ANGLE_UNIT ( ) SI_UNIT ( $, .RADIAN. ) );
#3168 = ORIENTED_EDGE ( 'NONE', *, *, #10986, .T. ) ;
#3169 = FACE_OUTER_BOUND ( 'NONE', #4143, .T. ) ;
#3170 = VERTEX_POINT ( 'NONE', #14616 ) ;
#3171 = ORIENTED_EDGE ( 'NONE', *, *, #6113, .F. ) ;
#3172 = CARTESIAN_POINT ( 'NONE',  ( 0.9108756637647450471, -6.979659189788935514, -6.219623095965384429 ) ) ;
#3173 = CARTESIAN_POINT ( 'NONE',  ( 628.4512226587627310, 156.2114428402112765, -209.9999999999999432 ) ) ;
#3174 = LINE ( 'NONE', #7677, #12028 ) ;
#3175 = EDGE_CURVE ( 'NONE', #4781, #6611, #11235, .T. ) ;
#3176 = CARTESIAN_POINT ( 'NONE',  ( -9.511508594537124495, 378.5275384125996538, -187.0000000000000284 ) ) ;
#3177 = ADVANCED_FACE ( 'NONE', ( #8818 ), #70, .F. ) ;
#3178 = FACE_OUTER_BOUND ( 'NONE', #11021, .T. ) ;
#3179 = VERTEX_POINT ( 'NONE', #5630 ) ;
#3180 = DIRECTION ( 'NONE',  ( -0.000000000000000000, -0.000000000000000000, 1.000000000000000000 ) ) ;
#3181 = DIRECTION ( 'NONE',  ( -1.000000000000000000, -7.930164461608254918E-15, 0.000000000000000000 ) ) ;
#3182 = ITEM_DEFINED_TRANSFORMATION ( 'NONE', 'NONE', #3356,  #9440 ) ;
#3183 = CARTESIAN_POINT ( 'NONE',  ( 112.9652219749295341, 376.5507399164317803, -210.0000000000000000 ) ) ;
#3184 = EDGE_LOOP ( 'NONE', ( #12737, #4793, #11521 ) ) ;
#3185 = B_SPLINE_CURVE_WITH_KNOTS ( 'NONE', 3,
 ( #278, #11504, #4593, #13877, #13654, #8049 ),
 .UNSPECIFIED., .F., .F.,
 ( 4, 2, 4 ),
 ( 4.336808689942017736E-19, 0.0002095117440864781224, 0.0004190234881729558111 ),
 .UNSPECIFIED. ) ;
#3186 = VERTEX_POINT ( 'NONE', #11096 ) ;
#3187 = CARTESIAN_POINT ( 'NONE',  ( -2.595115354961444076, -7.673029147243174641, -1.000000000000000000 ) ) ;
#3188 = EDGE_CURVE ( 'NONE', #8553, #5688, #9875, .T. ) ;
#3189 = LINE ( 'NONE', #13584, #3293 ) ;
#3190 = B_SPLINE_CURVE_WITH_KNOTS ( 'NONE', 3,
 ( #14112, #661, #1719, #746, #8503, #13085, #2969, #9767, #11890, #10720, #8646, #6363, #5330, #13227, #3121, #7463, #14264, #3042, #6512, #7625 ),
 .UNSPECIFIED., .F., .F.,
 ( 4, 2, 2, 2, 2, 2, 2, 2, 2, 4 ),
 ( 5.551115123125782702E-17, 0.001037574205614438111, 0.002075148411228820711, 0.003112722616843203310, 0.003631509719650373360, 0.004150296822457543409, 0.005187871028071766415, 0.006225445233685987685, 0.007263019439300210690, 0.008300593644914432828 ),
 .UNSPECIFIED. ) ;
#3191 = CARTESIAN_POINT ( 'NONE',  ( 1.399999999999999689, 9.062386313690412402E-16, 7.399999999999999467 ) ) ;
#3192 = ORIENTED_EDGE ( 'NONE', *, *, #12327, .F. ) ;
#3193 = CARTESIAN_POINT ( 'NONE',  ( -6.826296012759691223, -2.664253980652245168, -6.325071479460635970 ) ) ;
#3194 = ORIENTED_EDGE ( 'NONE', *, *, #6816, .T. ) ;
#3195 = DIRECTION ( 'NONE',  ( -9.794481010665704304E-16, -3.264827003555233190E-15, -1.000000000000000000 ) ) ;
#3196 = DIRECTION ( 'NONE',  ( 0.000000000000000000, 0.000000000000000000, 1.000000000000000000 ) ) ;
#3197 = DIRECTION ( 'NONE',  ( 0.000000000000000000, -0.5000000000000013323, -0.8660254037844380415 ) ) ;
#3198 = ORIENTED_EDGE ( 'NONE', *, *, #11207, .F. ) ;
#3199 = DIRECTION ( 'NONE',  ( 0.2873478855663437748, 0.9578262852211518741, 0.000000000000000000 ) ) ;
#3200 = ORIENTED_EDGE ( 'NONE', *, *, #12553, .F. ) ;
#3201 = ORIENTED_EDGE ( 'NONE', *, *, #12327, .T. ) ;
#3202 = DIRECTION ( 'NONE',  ( -0.000000000000000000, -0.000000000000000000, -1.000000000000000000 ) ) ;
#3203 = EDGE_CURVE ( 'NONE', #12661, #9848, #9030, .T. ) ;
#3204 = DIRECTION ( 'NONE',  ( 0.2873478855663452736, 0.9578262852211513190, 3.491481338843133355E-15 ) ) ;
#3205 = CARTESIAN_POINT ( 'NONE',  ( -5.560781378645575757, 6.809993116116508640E-16, -4.000000000000000000 ) ) ;
#3206 = EDGE_LOOP ( 'NONE', ( #1722, #5625, #10974, #1500, #5620 ) ) ;
#3207 = ORIENTED_EDGE ( 'NONE', *, *, #2889, .T. ) ;
#3208 = CARTESIAN_POINT ( 'NONE',  ( 6.245824673232968749, -4.939548505212512097, 1.655093584846542454 ) ) ;
#3209 = LINE ( 'NONE', #6606, #10371 ) ;
#3210 = CARTESIAN_POINT ( 'NONE',  ( 1.500000000000001332, 8.266365894244634333E-16, 6.750000000000000000 ) ) ;
#3211 = DIRECTION ( 'NONE',  ( -0.000000000000000000, -0.000000000000000000, -1.000000000000000000 ) ) ;
#3212 = CARTESIAN_POINT ( 'NONE',  ( 446.3084422793565409, 264.0194060144110608, -210.0000000000000000 ) ) ;
#3213 =( NAMED_UNIT ( * ) PLANE_ANGLE_UNIT ( ) SI_UNIT ( $, .RADIAN. ) );
#3214 = VERTEX_POINT ( 'NONE', #2227 ) ;
#3215 = EDGE_LOOP ( 'NONE', ( #2239, #14185, #10089, #6748 ) ) ;
#3216 = DIRECTION ( 'NONE',  ( 0.2873478855663502141, 0.9578262852211498757, -8.036520471939056366E-30 ) ) ;
#3217 = EDGE_CURVE ( 'NONE', #8002, #8575, #139, .T. ) ;
#3218 = ORIENTED_EDGE ( 'NONE', *, *, #10701, .T. ) ;
#3219 = DIRECTION ( 'NONE',  ( 0.000000000000000000, -0.000000000000000000, 1.000000000000000000 ) ) ;
#3220 = ADVANCED_FACE ( 'NONE', ( #5777 ), #4611, .T. ) ;
#3221 = CYLINDRICAL_SURFACE ( 'NONE', #4997, 4.000000000000000000 ) ;
#3222 = EDGE_CURVE ( 'NONE', #11200, #5805, #13535, .T. ) ;
#3223 = VERTEX_POINT ( 'NONE', #3421 ) ;
#3224 = DIRECTION ( 'NONE',  ( -1.000000000000000000, 0.000000000000000000, 0.000000000000000000 ) ) ;
#3225 = CARTESIAN_POINT ( 'NONE',  ( -0.5590169943749470072, 0.000000000000000000, 0.000000000000000000 ) ) ;
#3226 = EDGE_CURVE ( 'NONE', #6053, #8142, #1621, .T. ) ;
#3227 = PLANE ( 'NONE',  #6191 ) ;
#3228 = SHAPE_REPRESENTATION_RELATIONSHIP ( 'NONE' , 'NONE' ,  #2248, #12520 ) ;
#3229 = ORIENTED_EDGE ( 'NONE', *, *, #7212, .T. ) ;
#3230 = CARTESIAN_POINT ( 'NONE',  ( 640.0000000000000000, 160.0000000000000284, 210.0000000000000000 ) ) ;
#3231 = ORIENTED_EDGE ( 'NONE', *, *, #9010, .F. ) ;
#3232 = ORIENTED_EDGE ( 'NONE', *, *, #9647, .F. ) ;
#3233 = CARTESIAN_POINT ( 'NONE',  ( 611.4942090049448780, 232.4210031920598283, 184.7999999999999829 ) ) ;
#3234 = CARTESIAN_POINT ( 'NONE',  ( 628.9938615732160088, 155.3996772905950081, -210.0000000000000000 ) ) ;
#3235 = ADVANCED_FACE ( 'NONE', ( #2293 ), #3043, .F. ) ;
#3236 = CARTESIAN_POINT ( 'NONE',  ( 6.499999999999999112, -1.280811194704859490, -0.07768058122908397256 ) ) ;
#3237 = AXIS2_PLACEMENT_3D ( 'NONE', #4735, #9226, #416 ) ;
#3238 = VECTOR ( 'NONE', #5953, 1000.000000000000114 ) ;
#3239 = DIRECTION ( 'NONE',  ( -0.000000000000000000, -0.000000000000000000, -1.000000000000000000 ) ) ;
#3240 = CARTESIAN_POINT ( 'NONE',  ( 0.1597025669806095838, 1.557591170363294975, -4.000000000000000000 ) ) ;
#3241 = CARTESIAN_POINT ( 'NONE',  ( 629.0000000000000000, 166.0000000000000284, 187.5000000000000000 ) ) ;
#3242 = CARTESIAN_POINT ( 'NONE',  ( 641.0000000000000000, 154.0000000000000568, -187.5000000000000000 ) ) ;
#3243 = ORIENTED_EDGE ( 'NONE', *, *, #2297, .T. ) ;
#3244 = CARTESIAN_POINT ( 'NONE',  ( 650.0000000000000000, 145.0000000000000568, -190.0000000000000000 ) ) ;
#3245 = LINE ( 'NONE', #5471, #14359 ) ;
#3246 = APPLICATION_PROTOCOL_DEFINITION ( 'draft international standard', 'automotive_design', 1998, #7544 ) ;
#3247=STYLED_ITEM('',(#14681),#2529);
#3248 = CARTESIAN_POINT ( 'NONE',  ( -3.399999999999999911, 4.163799117101000559E-16, -8.000000000000000000 ) ) ;
#3249 = EDGE_CURVE ( 'NONE', #5903, #4614, #9654, .T. ) ;
#3250 = AXIS2_PLACEMENT_3D ( 'NONE', #3727, #230, #3809 ) ;
#3251 = ORIENTED_EDGE ( 'NONE', *, *, #4308, .T. ) ;
#3252 = ORIENTED_EDGE ( 'NONE', *, *, #349, .F. ) ;
#3253 = DIRECTION ( 'NONE',  ( 1.000000000000000000, 9.498873539028489960E-17, 0.000000000000000000 ) ) ;
#3254 = EDGE_CURVE ( 'NONE', #7536, #5493, #9993, .T. ) ;
#3255 = LINE ( 'NONE', #2364, #12230 ) ;
#3256 = CARTESIAN_POINT ( 'NONE',  ( -2.241046694639089232, 6.576374040525770681, -6.171384342982497273 ) ) ;
#3258 = EDGE_LOOP ( 'NONE', ( #1543, #7786, #6655, #9287 ) ) ;
#3257 = COLOUR_RGB ( '',1.000000000000000000, 0.9490196078431372140, 0.9098039215686274384 ) ;
#3259 = VECTOR ( 'NONE', #13471, 1000.000000000000000 ) ;
#3260 = UNCERTAINTY_MEASURE_WITH_UNIT (LENGTH_MEASURE( 1.000000000000000082E-05 ), #9668, 'distance_accuracy_value', 'NONE');
#3261 = PLANE ( 'NONE',  #1247 ) ;
#3262 = ORIENTED_EDGE ( 'NONE', *, *, #7448, .T. ) ;
#3263 = LINE ( 'NONE', #8654, #8679 ) ;
#3264 = DIRECTION ( 'NONE',  ( -0.000000000000000000, -0.000000000000000000, -1.000000000000000000 ) ) ;
#3265 = CARTESIAN_POINT ( 'NONE',  ( 470.8287951810180516, 310.9528939902474463, -210.0000000000000000 ) ) ;
#3266 = ORIENTED_EDGE ( 'NONE', *, *, #13723, .F. ) ;
#3267 = ORIENTED_EDGE ( 'NONE', *, *, #13640, .F. ) ;
#3268 = DIRECTION ( 'NONE',  ( 0.000000000000000000, 0.000000000000000000, 1.000000000000000000 ) ) ;
#3269 = VECTOR ( 'NONE', #5844, 1000.000000000000000 ) ;
#3270 = AXIS2_PLACEMENT_3D ( 'NONE', #12259, #6671, #4530 ) ;
#3271 = CARTESIAN_POINT ( 'NONE',  ( -0.1481481481481481122, -4.797713218419819903, -1.000000000000000000 ) ) ;
#3272 = VECTOR ( 'NONE', #10474, 1000.000000000000000 ) ;
#3273 = DIRECTION ( 'NONE',  ( 0.000000000000000000, 0.000000000000000000, -1.000000000000000000 ) ) ;
#3274=STYLED_ITEM('',(#14667),#7155);
#3275 = EDGE_LOOP ( 'NONE', ( #5788, #13853, #13254, #3732, #11465, #10434, #1172, #8641 ) ) ;
#3276 = ORIENTED_EDGE ( 'NONE', *, *, #8006, .T. ) ;
#3277 = CARTESIAN_POINT ( 'NONE',  ( 8.500000000000000000, 5.773502691896261751, -2.749426538070115714E-16 ) ) ;
#3278 = EDGE_CURVE ( 'NONE', #2328, #248, #11283, .T. ) ;
#3279 = DIRECTION ( 'NONE',  ( -1.000000000000000000, -0.000000000000000000, -0.000000000000000000 ) ) ;
#3280 = AXIS2_PLACEMENT_3D ( 'NONE', #12994, #2886, #7385 ) ;
#3281 = CIRCLE ( 'NONE', #8216, 2.055000000000000160 ) ;
#3282 = CARTESIAN_POINT ( 'NONE',  ( -0.5469614295416921346, 4.303013824936271270, -3.535263753543735454 ) ) ;
#3283 = LINE ( 'NONE', #11108, #158 ) ;
#3284 = LINE ( 'NONE', #150, #13745 ) ;
#3285 = FILL_AREA_STYLE_COLOUR ( '', #10178 ) ;
#3286 = ORIENTED_EDGE ( 'NONE', *, *, #5552, .F. ) ;
#3287 = CYLINDRICAL_SURFACE ( 'NONE', #697, 5.750000000000000000 ) ;
#3288 = ORIENTED_EDGE ( 'NONE', *, *, #14406, .F. ) ;
#3289 = VERTEX_POINT ( 'NONE', #10280 ) ;
#3290 = FACE_OUTER_BOUND ( 'NONE', #8079, .T. ) ;
#3291 = PRESENTATION_LAYER_ASSIGNMENT (  '', '', ( #3274 ) ) ;
#3292 = ORIENTED_EDGE ( 'NONE', *, *, #10269, .T. ) ;
#3293 = VECTOR ( 'NONE', #7908, 1000.000000000000000 ) ;
#3294 = AXIS2_PLACEMENT_3D ( 'NONE', #7464, #530, #1562 ) ;
#3295 = CARTESIAN_POINT ( 'NONE',  ( 0.000000000000000000, 0.000000000000000000, -5.000000000000000888 ) ) ;
#3296 = APPLICATION_CONTEXT ( 'automotive_design' ) ;
#3297 = CARTESIAN_POINT ( 'NONE',  ( 0.04201760816083372624, -0.9730571234388146751, 4.999999999999997335 ) ) ;
#3298 = EDGE_LOOP ( 'NONE', ( #3194, #14214 ) ) ;
#3299 = DIRECTION ( 'NONE',  ( 0.000000000000000000, 1.000000000000000000, 0.000000000000000000 ) ) ;
#3300 = ADVANCED_FACE ( 'NONE', ( #12267 ), #7281, .T. ) ;
#3301 = DIRECTION ( 'NONE',  ( 0.000000000000000000, 0.000000000000000000, -1.000000000000000000 ) ) ;
#3302 = CIRCLE ( 'NONE', #6367, 2.649999999999985700 ) ;
#3303 = CARTESIAN_POINT ( 'NONE',  ( -0.5204879950542059541, -7.205049615410630715, -0.5609245978742286587 ) ) ;
#3304 = DIRECTION ( 'NONE',  ( -1.000000000000000000, -0.000000000000000000, -0.000000000000000000 ) ) ;
#3305 = ORIENTED_EDGE ( 'NONE', *, *, #7056, .F. ) ;
#3306 = ADVANCED_FACE ( 'NONE', ( #4382 ), #8877, .F. ) ;
#3307 = AXIS2_PLACEMENT_3D ( 'NONE', #6924, #1311, #1812 ) ;
#3308 =( LENGTH_UNIT ( ) NAMED_UNIT ( * ) SI_UNIT ( .MILLI., .METRE. ) );
#3309 = EDGE_LOOP ( 'NONE', ( #780, #9205, #13000, #1149 ) ) ;
#3310 = EDGE_CURVE ( 'NONE', #4698, #10509, #3517, .T. ) ;
#3311 = ORIENTED_EDGE ( 'NONE', *, *, #10418, .F. ) ;
#3313 = DIRECTION ( 'NONE',  ( 1.000000000000000000, 9.498873539028489960E-17, 0.000000000000000000 ) ) ;
#3312 = VECTOR ( 'NONE', #4594, 1000.000000000000114 ) ;
#3314 = AXIS2_PLACEMENT_3D ( 'NONE', #12388, #5690, #10192 ) ;
#3315 = EDGE_CURVE ( 'NONE', #734, #5738, #13462, .T. ) ;
#3316 = DIRECTION ( 'NONE',  ( 0.000000000000000000, 0.000000000000000000, 1.000000000000000000 ) ) ;
#3318 = VECTOR ( 'NONE', #5866, 1000.000000000000000 ) ;
#3317 = LINE ( 'NONE', #2261, #3087 ) ;
#3319 = AXIS2_PLACEMENT_3D ( 'NONE', #598, #2974, #14202 ) ;
#3320 = FACE_OUTER_BOUND ( 'NONE', #1282, .T. ) ;
#3321 = DIRECTION ( 'NONE',  ( 1.000000000000000000, 0.000000000000000000, 0.000000000000000000 ) ) ;
#3322 = FACE_OUTER_BOUND ( 'NONE', #7315, .T. ) ;
#3323 = AXIS2_PLACEMENT_3D ( 'NONE', #4885, #13882, #2666 ) ;
#3324 = CARTESIAN_POINT ( 'NONE',  ( 0.2500000000000002220, 5.204748896376250699E-16, -4.250000000000000000 ) ) ;
#3325 = ORIENTED_EDGE ( 'NONE', *, *, #3339, .T. ) ;
#3326 = VECTOR ( 'NONE', #6616, 1000.000000000000000 ) ;
#3327 = FACE_OUTER_BOUND ( 'NONE', #14566, .T. ) ;
#3328 = CARTESIAN_POINT ( 'NONE',  ( 2.500000000000000000, -1.178949249685214307, 2.042000000000001592 ) ) ;
#3329 = ITEM_DEFINED_TRANSFORMATION ( 'NONE', 'NONE', #11588,  #9440 ) ;
#3330 = ADVANCED_FACE ( 'NONE', ( #3575 ), #1638, .F. ) ;
#3331 = VECTOR ( 'NONE', #14496, 1000.000000000000000 ) ;
#3332 = EDGE_CURVE ( 'NONE', #11582, #1364, #13645, .T. ) ;
#3333 = CARTESIAN_POINT ( 'NONE',  ( 443.6584422793565636, 264.0194060144110608, 190.0000000000000000 ) ) ;
#3334 = COLOUR_RGB ( '',0.8941176470588234615, 0.8941176470588234615, 0.8941176470588234615 ) ;
#3335 = ORIENTED_EDGE ( 'NONE', *, *, #130, .F. ) ;
#3336 = VERTEX_POINT ( 'NONE', #1561 ) ;
#3337 = DIRECTION ( 'NONE',  ( -0.000000000000000000, -0.000000000000000000, 1.000000000000000000 ) ) ;
#3338 = DIRECTION ( 'NONE',  ( -0.2873478855663453846, -0.9578262852211513190, 0.000000000000000000 ) ) ;
#3339 = EDGE_CURVE ( 'NONE', #4895, #2075, #1498, .T. ) ;
#3340 = LINE ( 'NONE', #12328, #446 ) ;
#3341 = AXIS2_PLACEMENT_3D ( 'NONE', #9055, #12433, #2187 ) ;
#3342 = CIRCLE ( 'NONE', #11349, 2.649999999999985700 ) ;
#3343 = PRODUCT_DEFINITION_SHAPE ( 'NONE', 'NONE',  #9297 ) ;
#3344 = LINE ( 'NONE', #5545, #2125 ) ;
#3345 = ORIENTED_EDGE ( 'NONE', *, *, #3332, .F. ) ;
#3346 = CARTESIAN_POINT ( 'NONE',  ( 610.0000000000000000, 227.4403065089105951, -187.0000000000000000 ) ) ;
#3347 = EDGE_LOOP ( 'NONE', ( #12243, #4572 ) ) ;
#3348 = LINE ( 'NONE', #1942, #7742 ) ;
#3349 = FACE_OUTER_BOUND ( 'NONE', #10900, .T. ) ;
#3350 = FILL_AREA_STYLE ('',( #13530 ) ) ;
#3351 = CIRCLE ( 'NONE', #7344, 2.200000000000009948 ) ;
#3352 = PLANE ( 'NONE',  #12740 ) ;
#3353 = ORIENTED_EDGE ( 'NONE', *, *, #5219, .F. ) ;
#3354 = ORIENTED_EDGE ( 'NONE', *, *, #8629, .F. ) ;
#3355 = CARTESIAN_POINT ( 'NONE',  ( -1.747541505913277282, 3.837784562140256650, -3.503702292528906526 ) ) ;
#3356 = AXIS2_PLACEMENT_3D ( 'NONE', #10424, #13890, #3643 ) ;
#3357 = CARTESIAN_POINT ( 'NONE',  ( 2.999999999999999112, -2.309401076758502480, -4.000000000000000000 ) ) ;
#3358 = PLANE ( 'NONE',  #4271 ) ;
#3359 = CIRCLE ( 'NONE', #12298, 7.900000000000002132 ) ;
#3360 = EDGE_LOOP ( 'NONE', ( #12829, #10464, #1050, #8476, #9983 ) ) ;
#3361 = ORIENTED_EDGE ( 'NONE', *, *, #3492, .T. ) ;
#3362 = FACE_OUTER_BOUND ( 'NONE', #1541, .T. ) ;
#3363 = CARTESIAN_POINT ( 'NONE',  ( 0.6448876103708359731, 4.246476118072354922, -0.2256878752776725616 ) ) ;
#3364 = AXIS2_PLACEMENT_3D ( 'NONE', #9317, #12854, #7237 ) ;
#3365 = LINE ( 'NONE', #14442, #652 ) ;
#3366 = FACE_OUTER_BOUND ( 'NONE', #5624, .T. ) ;
#3367 = DIRECTION ( 'NONE',  ( -0.000000000000000000, -0.000000000000000000, 1.000000000000000000 ) ) ;
#3368 = VERTEX_POINT ( 'NONE', #7178 ) ;
#3369 = DIRECTION ( 'NONE',  ( 0.000000000000000000, 0.000000000000000000, -1.000000000000000000 ) ) ;
#3370 = ORIENTED_EDGE ( 'NONE', *, *, #7769, .T. ) ;
#3371 = ORIENTED_EDGE ( 'NONE', *, *, #3711, .F. ) ;
#3372 = CIRCLE ( 'NONE', #11838, 0.7499999999999997780 ) ;
#3373 = DIRECTION ( 'NONE',  ( 0.000000000000000000, 0.000000000000000000, 1.000000000000000000 ) ) ;
#3374 = CIRCLE ( 'NONE', #5962, 4.000000000000000000 ) ;
#3375 = ORIENTED_EDGE ( 'NONE', *, *, #13140, .T. ) ;
#3376 = EDGE_CURVE ( 'NONE', #13812, #1030, #11050, .T. ) ;
#3377 = EDGE_CURVE ( 'NONE', #1238, #1371, #4765, .T. ) ;
#3378 = CARTESIAN_POINT ( 'NONE',  ( 1.500000000000001332, 0.000000000000000000, 0.000000000000000000 ) ) ;
#3379 = PLANE ( 'NONE',  #12518 ) ;
#3380 = ORIENTED_EDGE ( 'NONE', *, *, #10973, .F. ) ;
#3381 = DIRECTION ( 'NONE',  ( 1.000000000000000000, 0.000000000000000000, 0.000000000000000000 ) ) ;
#3382 = DIRECTION ( 'NONE',  ( -0.9578262852210943645, 0.2873478855665353993, 0.000000000000000000 ) ) ;
#3383 = AXIS2_PLACEMENT_3D ( 'NONE', #3722, #667, #1642 ) ;
#3384 = DIRECTION ( 'NONE',  ( -0.9578262852211507639, 0.2873478855663477716, 0.000000000000000000 ) ) ;
#3385 = SURFACE_STYLE_FILL_AREA ( #2414 ) ;
#3386 = ORIENTED_EDGE ( 'NONE', *, *, #1824, .T. ) ;
#3387 = CARTESIAN_POINT ( 'NONE',  ( 635.0000000000000000, 160.0000000000000284, -215.9978484569338946 ) ) ;
#3388 = ORIENTED_EDGE ( 'NONE', *, *, #3766, .F. ) ;
#3389 = EDGE_LOOP ( 'NONE', ( #13562, #1154, #5348 ) ) ;
#3390 = CYLINDRICAL_SURFACE ( 'NONE', #10804, 4.199999999999926459 ) ;
#3391 = EDGE_CURVE ( 'NONE', #12373, #5236, #12571, .T. ) ;
#3392 = SHAPE_REPRESENTATION ( 'plain washer 10669 type nl_iso_ISO 10669-5.4-N', ( #9440 ), #13 ) ;
#3393 = CARTESIAN_POINT ( 'NONE',  ( 627.6905843535678287, 158.0483056743123882, -210.0000000000000284 ) ) ;
#3394 = CARTESIAN_POINT ( 'NONE',  ( 4.211140560182196957, -2.431303136016555122, -3.745885042887436622 ) ) ;
#3395 = DIRECTION ( 'NONE',  ( 0.000000000000000000, 0.000000000000000000, 1.000000000000000000 ) ) ;
#3396 = EDGE_CURVE ( 'NONE', #11414, #54, #4679, .T. ) ;
#3397 = CARTESIAN_POINT ( 'NONE',  ( 20.55500000000001748, 0.000000000000000000, 2.500000000000000888 ) ) ;
#3398 = CARTESIAN_POINT ( 'NONE',  ( 0.000000000000000000, 0.000000000000000000, -225.5000000000000000 ) ) ;
#3399 = CARTESIAN_POINT ( 'NONE',  ( 448.9584422793565750, 264.0194060144110608, -187.0000000000000000 ) ) ;
#3400 = EDGE_LOOP ( 'NONE', ( #13181, #11347, #12872 ) ) ;
#3401 = LINE ( 'NONE', #2351, #13616 ) ;
#3402 = CARTESIAN_POINT ( 'NONE',  ( 6.367873360227556567, 2.886751345948122882, -5.000000000000000000 ) ) ;
#3403 = CARTESIAN_POINT ( 'NONE',  ( -6.500000000000002665, -2.501851166488385125, -5.848636054922036642 ) ) ;
#3404 = ORIENTED_EDGE ( 'NONE', *, *, #9376, .T. ) ;
#3405 = ORIENTED_EDGE ( 'NONE', *, *, #1576, .F. ) ;
#3406 = DIRECTION ( 'NONE',  ( -0.9578262852211507639, 0.2873478855663477716, 0.000000000000000000 ) ) ;
#3407 = EDGE_CURVE ( 'NONE', #54, #352, #11526, .T. ) ;
#3408 = DIRECTION ( 'NONE',  ( -0.000000000000000000, -0.000000000000000000, 1.000000000000000000 ) ) ;
#3409 = EDGE_CURVE ( 'NONE', #4509, #4487, #5603, .T. ) ;
#3410 = CARTESIAN_POINT ( 'NONE',  ( -9.999999999999840128, 413.4403065089115330, -184.7999999999999829 ) ) ;
#3411 = EDGE_CURVE ( 'NONE', #503, #214, #10350, .T. ) ;
#3412 = CARTESIAN_POINT ( 'NONE',  ( 0.000000000000000000, 0.000000000000000000, 0.000000000000000000 ) ) ;
#3413 = EDGE_LOOP ( 'NONE', ( #11370, #10060, #9371, #14454 ) ) ;
#3414 = EDGE_CURVE ( 'NONE', #3596, #7551, #11604, .T. ) ;
#3415 = PLANE ( 'NONE',  #5389 ) ;
#3416 = CARTESIAN_POINT ( 'NONE',  ( 639.0000000000000000, 156.0000000000000000, -225.5000000000000000 ) ) ;
#3417 = DIRECTION ( 'NONE',  ( 1.000000000000000000, 0.000000000000000000, 0.000000000000000000 ) ) ;
#3418 = ORIENTED_EDGE ( 'NONE', *, *, #297, .F. ) ;
#3419 = VERTEX_POINT ( 'NONE', #11733 ) ;
#3420 = CARTESIAN_POINT ( 'NONE',  ( -0.6937372685066653943, 4.453844082567723461, -3.610536846335889116 ) ) ;
#3421 = CARTESIAN_POINT ( 'NONE',  ( 144.7991633467111683, 386.6211705227183870, 190.0000000000000568 ) ) ;
#3422 = DIRECTION ( 'NONE',  ( 0.2873478855663477161, 0.9578262852211506528, 0.000000000000000000 ) ) ;
#3423 = B_SPLINE_CURVE_WITH_KNOTS ( 'NONE', 3,
 ( #9898, #7689, #8799, #13225, #12172, #2968 ),
 .UNSPECIFIED., .F., .F.,
 ( 4, 2, 4 ),
 ( 0.003841072314098365435, 0.005765657563962188134, 0.007690242813826009965 ),
 .UNSPECIFIED. ) ;
#3424 = VERTEX_POINT ( 'NONE', #6067 ) ;
#3425 = ORIENTED_EDGE ( 'NONE', *, *, #426, .F. ) ;
#3426 = CARTESIAN_POINT ( 'NONE',  ( 609.8754609228352592, 185.7164421964179439, -185.4807968138250374 ) ) ;
#3427 = DIRECTION ( 'NONE',  ( 0.000000000000000000, 0.000000000000000000, -1.000000000000000000 ) ) ;
#3428 = CYLINDRICAL_SURFACE ( 'NONE', #4683, 4.199999999999926459 ) ;
#3429 = CARTESIAN_POINT ( 'NONE',  ( 641.0000000000000000, 166.0000000000000284, 187.5000000000000000 ) ) ;
#3430 = VERTEX_POINT ( 'NONE', #11452 ) ;
#3431 = DIRECTION ( 'NONE',  ( -1.000000000000000000, 0.000000000000000000, 0.000000000000000000 ) ) ;
#3432 = ORIENTED_EDGE ( 'NONE', *, *, #2963, .F. ) ;
#3433 = ORIENTED_EDGE ( 'NONE', *, *, #8898, .F. ) ;
#3434 = DIRECTION ( 'NONE',  ( -1.000000000000000000, 0.000000000000000000, 0.000000000000000000 ) ) ;
#3435 = EDGE_CURVE ( 'NONE', #11448, #4487, #5869, .T. ) ;
#3436 = ORIENTED_EDGE ( 'NONE', *, *, #5552, .T. ) ;
#3437 = EDGE_CURVE ( 'NONE', #8013, #604, #4977, .T. ) ;
#3438 = CARTESIAN_POINT ( 'NONE',  ( -4.336808689942017736E-16, 7.505553499465137612, -0.8000000000000003775 ) ) ;
#3439 = FACE_OUTER_BOUND ( 'NONE', #5993, .T. ) ;
#3440 = ORIENTED_EDGE ( 'NONE', *, *, #11928, .T. ) ;
#3441 = DIRECTION ( 'NONE',  ( -1.000000000000000000, -0.000000000000000000, 0.000000000000000000 ) ) ;
#3442 = DIRECTION ( 'NONE',  ( 0.000000000000000000, 0.000000000000000000, -1.000000000000000000 ) ) ;
#3443 = CYLINDRICAL_SURFACE ( 'NONE', #2524, 2.200000000000007283 ) ;
#3444 = CARTESIAN_POINT ( 'NONE',  ( -20.63749999999999929, 0.000000000000000000, 0.000000000000000000 ) ) ;
#3445 = ORIENTED_EDGE ( 'NONE', *, *, #9574, .T. ) ;
#3447 = ADVANCED_FACE ( 'NONE', ( #9478 ), #7520, .F. ) ;
#3446 = LINE ( 'NONE', #13495, #9425 ) ;
#3448 = VERTEX_POINT ( 'NONE', #5053 ) ;
#3449 = B_SPLINE_CURVE_WITH_KNOTS ( 'NONE', 3,
 ( #13238, #10946, #821, #4234, #8588, #10797, #5196, #7634, #14205, #7332 ),
 .UNSPECIFIED., .F., .F.,
 ( 4, 2, 2, 2, 4 ),
 ( 0.000000000000000000, 0.001989602278884366159, 0.003979204557768732317, 0.005968806836653096741, 0.007958409115537461165 ),
 .UNSPECIFIED. ) ;
#3450 = ORIENTED_EDGE ( 'NONE', *, *, #12173, .F. ) ;
#3451 = CARTESIAN_POINT ( 'NONE',  ( 443.6584422793565636, 264.0194060144110608, -210.0000000000000000 ) ) ;
#3452 = PRODUCT_DEFINITION_SHAPE ( 'NONE', 'NONE',  #1603 ) ;
#3453 = DIRECTION ( 'NONE',  ( 1.000000000000000000, 0.000000000000000000, 0.000000000000000000 ) ) ;
#3454 = CARTESIAN_POINT ( 'NONE',  ( 4.000000000000000000, 0.000000000000000000, 0.000000000000000000 ) ) ;
#3455 = EDGE_CURVE ( 'NONE', #5297, #12569, #1026, .T. ) ;
#3456 = LINE ( 'NONE', #12448, #11804 ) ;
#3457 = LINE ( 'NONE', #6855, #7359 ) ;
#3458 = DIRECTION ( 'NONE',  ( -1.000000000000000000, -0.000000000000000000, -0.000000000000000000 ) ) ;
#3459 = DIRECTION ( 'NONE',  ( 1.000000000000000000, -0.000000000000000000, 0.000000000000000000 ) ) ;
#3460 = EDGE_CURVE ( 'NONE', #11959, #4981, #9610, .T. ) ;
#3461 = ORIENTED_EDGE ( 'NONE', *, *, #7550, .T. ) ;
#3462 = LINE ( 'NONE', #11427, #6116 ) ;
#3463 = CARTESIAN_POINT ( 'NONE',  ( 2.999999999999999112, 0.000000000000000000, 0.000000000000000000 ) ) ;
#3464 = DIRECTION ( 'NONE',  ( 1.000000000000000000, 0.000000000000000000, -0.000000000000000000 ) ) ;
#3465 = APPLICATION_PROTOCOL_DEFINITION ( 'draft international standard', 'automotive_design', 1998, #14428 ) ;
#3466 = ORIENTED_EDGE ( 'NONE', *, *, #13862, .F. ) ;
#3467 = B_SPLINE_CURVE_WITH_KNOTS ( 'NONE', 3,
 ( #4824, #6949, #3925, #1491, #9245, #10423, #5989, #12780 ),
 .UNSPECIFIED., .F., .F.,
 ( 4, 2, 2, 4 ),
 ( 2.465131517390770070E-07, 0.001183067374689869946, 0.001774477805458935659, 0.002365888236228001588 ),
 .UNSPECIFIED. ) ;
#3468 = CARTESIAN_POINT ( 'NONE',  ( 6.500000000000000000, 3.752776749732564365, -6.177805531629060987 ) ) ;
#3469 = ORIENTED_EDGE ( 'NONE', *, *, #6926, .T. ) ;
#3470 = ORIENTED_EDGE ( 'NONE', *, *, #3680, .T. ) ;
#3471 = CARTESIAN_POINT ( 'NONE',  ( 6.500000000000000000, -3.752776749732574135, -6.064240316920400886 ) ) ;
#3472 = CARTESIAN_POINT ( 'NONE',  ( 639.0000000000000000, 164.0000000000000000, -233.5000000000000000 ) ) ;
#3473 = VECTOR ( 'NONE', #8121, 1000.000000000000000 ) ;
#3474 = VECTOR ( 'NONE', #733, 1000.000000000000227 ) ;
#3476 = CARTESIAN_POINT ( 'NONE',  ( 6.534838248920896930, -2.951765777552407766, 5.112608298763836601 ) ) ;
#3475 = CIRCLE ( 'NONE', #14545, 5.560781378645573980 ) ;
#3477 = DIRECTION ( 'NONE',  ( -1.000000000000000000, -6.938893903907222067E-15, 0.000000000000000000 ) ) ;
#3478 = CARTESIAN_POINT ( 'NONE',  ( 6.541334219041339715, -5.921300567812619597, 0.03049376373817746025 ) ) ;
#3479 = ADVANCED_FACE ( 'NONE', ( #13013 ), #813, .F. ) ;
#3480 = ORIENTED_EDGE ( 'NONE', *, *, #7191, .T. ) ;
#3481 = COLOUR_RGB ( '',1.000000000000000000, 0.9490196078431372140, 0.9098039215686274384 ) ;
#3482 = DIRECTION ( 'NONE',  ( -1.000000000000000000, 0.000000000000000000, 0.000000000000000000 ) ) ;
#3483 = CARTESIAN_POINT ( 'NONE',  ( 635.0000000000000000, 160.0000000000000284, -233.5000000000000000 ) ) ;
#3484 = ADVANCED_FACE ( 'NONE', ( #11954 ), #7320, .T. ) ;
#3485 = CARTESIAN_POINT ( 'NONE',  ( 6.367873360227558344, 5.773502691896261751, 0.000000000000000000 ) ) ;
#3486 = EDGE_LOOP ( 'NONE', ( #4129, #8614, #10605, #6105 ) ) ;
#3487 = ORIENTED_EDGE ( 'NONE', *, *, #34, .T. ) ;
#3488 = CARTESIAN_POINT ( 'NONE',  ( 627.5000000000000000, 160.0000000000000284, -207.0000000000000000 ) ) ;
#3489 = EDGE_CURVE ( 'NONE', #12842, #6920, #4009, .T. ) ;
#3490 = DIRECTION ( 'NONE',  ( -1.000000000000000000, -0.000000000000000000, -0.000000000000000000 ) ) ;
#3491 = COLOUR_RGB ( '',1.000000000000000000, 0.9490196078431372140, 0.9098039215686274384 ) ;
#3492 = EDGE_CURVE ( 'NONE', #13350, #2075, #3190, .T. ) ;
#3493 = CARTESIAN_POINT ( 'NONE',  ( 6.541171661047877173, 5.920857802016177729, 0.02973393389965222483 ) ) ;
#3494 = VECTOR ( 'NONE', #10879, 1000.000000000000000 ) ;
#3495 = ORIENTED_EDGE ( 'NONE', *, *, #6109, .F. ) ;
#3496 = ORIENTED_EDGE ( 'NONE', *, *, #13714, .T. ) ;
#3497 = CARTESIAN_POINT ( 'NONE',  ( 610.2340919441475080, 189.6262799281293212, -186.5592670532760167 ) ) ;
#3498 = CARTESIAN_POINT ( 'NONE',  ( 1.734723475976807094E-15, 4.618802153517012954, -0.4999999999999995559 ) ) ;
#3499 = DIRECTION ( 'NONE',  ( -0.000000000000000000, -0.000000000000000000, -1.000000000000000000 ) ) ;
#3500 = PLANE ( 'NONE',  #5595 ) ;
#3501 = PLANE ( 'NONE',  #4563 ) ;
#3502 = VERTEX_POINT ( 'NONE', #7543 ) ;
#3503 = AXIS2_PLACEMENT_3D ( 'NONE', #11873, #642, #14030 ) ;
#3504 = CARTESIAN_POINT ( 'NONE',  ( 0.000000000000000000, 0.000000000000000000, 0.000000000000000000 ) ) ;
#3505 = VECTOR ( 'NONE', #3197, 999.9999999999997726 ) ;
#3506 = VECTOR ( 'NONE', #11881, 1000.000000000000114 ) ;
#3507 = ORIENTED_EDGE ( 'NONE', *, *, #4667, .T. ) ;
#3508 = VERTEX_POINT ( 'NONE', #9546 ) ;
#3509 = CARTESIAN_POINT ( 'NONE',  ( 636.7009106935324780, 155.5114698605638637, 210.0000000000000000 ) ) ;
#3510 = EDGE_CURVE ( 'NONE', #4895, #7124, #12931, .T. ) ;
#3511 = EDGE_CURVE ( 'NONE', #10831, #14275, #1932, .T. ) ;
#3512 = ORIENTED_EDGE ( 'NONE', *, *, #8612, .T. ) ;
#3513 = AXIS2_PLACEMENT_3D ( 'NONE', #6996, #9074, #1477 ) ;
#3514 = ADVANCED_FACE ( 'NONE', ( #5114, #12110 ), #14049, .F. ) ;
#3515 = CARTESIAN_POINT ( 'NONE',  ( -1.250000000000000000, -6.429618962271402616, -1.000000000000000000 ) ) ;
#3516 = CARTESIAN_POINT ( 'NONE',  ( 629.7500000000000000, 160.0000000000000284, -190.0000000000000000 ) ) ;
#3517 = CIRCLE ( 'NONE', #432, 4.199999999999926459 ) ;
#3518 = AXIS2_PLACEMENT_3D ( 'NONE', #3033, #5391, #6272 ) ;
#3519 = ORIENTED_EDGE ( 'NONE', *, *, #4856, .F. ) ;
#3520 = DIRECTION ( 'NONE',  ( -0.000000000000000000, 0.000000000000000000, -1.000000000000000000 ) ) ;
#3521 = CARTESIAN_POINT ( 'NONE',  ( 2.500000000000000888, 3.061616997868384127E-16, -4.974599999999998801 ) ) ;
#3522 = DIRECTION ( 'NONE',  ( 0.000000000000000000, 0.000000000000000000, 1.000000000000000000 ) ) ;
#3523 = DIRECTION ( 'NONE',  ( -1.000000000000000000, 0.000000000000000000, 0.000000000000000000 ) ) ;
#3524 =( LENGTH_UNIT ( ) NAMED_UNIT ( * ) SI_UNIT ( .MILLI., .METRE. ) );
#3525 = ORIENTED_EDGE ( 'NONE', *, *, #13842, .F. ) ;
#3526 = CIRCLE ( 'NONE', #3988, 4.000000000000000000 ) ;
#3527 = DIRECTION ( 'NONE',  ( 0.000000000000000000, 0.000000000000000000, 1.000000000000000000 ) ) ;
#3528 = ORIENTED_EDGE ( 'NONE', *, *, #4783, .T. ) ;
#3529 = CIRCLE ( 'NONE', #5415, 7.399999999999999467 ) ;
#3530 = AXIS2_PLACEMENT_3D ( 'NONE', #4010, #12862, #4093 ) ;
#3531 = VERTEX_POINT ( 'NONE', #9693 ) ;
#3532 = FACE_OUTER_BOUND ( 'NONE', #7190, .T. ) ;
#3533 = DIRECTION ( 'NONE',  ( 0.000000000000000000, -1.000000000000000000, 0.000000000000000000 ) ) ;
#3534 = VECTOR ( 'NONE', #13559, 1000.000000000000000 ) ;
#3535 = LINE ( 'NONE', #104, #484 ) ;
#3536 = DIRECTION ( 'NONE',  ( -0.9578262852211514300, 0.2873478855663454401, 0.000000000000000000 ) ) ;
#3537 = CIRCLE ( 'NONE', #1645, 5.000000000000004441 ) ;
#3538 = CIRCLE ( 'NONE', #1646, 4.000000000000000000 ) ;
#3539 = DIRECTION ( 'NONE',  ( 0.000000000000000000, 1.224646799147353207E-16, 1.000000000000000000 ) ) ;
#3540 = CARTESIAN_POINT ( 'NONE',  ( 124.4591373975826230, 414.8637913252775888, 0.000000000000000000 ) ) ;
#3541 = CARTESIAN_POINT ( 'NONE',  ( 4.078421086530217288, -3.990950201428958621, -1.000000000000000000 ) ) ;
#3542 = EDGE_LOOP ( 'NONE', ( #14226, #8608, #2334, #8662 ) ) ;
#3543 = DIRECTION ( 'NONE',  ( 0.000000000000000000, 0.000000000000000000, 1.000000000000000000 ) ) ;
#3544 = DIRECTION ( 'NONE',  ( 1.000000000000000000, 0.000000000000000000, 0.000000000000000000 ) ) ;
#3545 = CARTESIAN_POINT ( 'NONE',  ( 610.8620436566991430, 188.5525593289319488, 184.8000000000000398 ) ) ;
#3546 = ITEM_DEFINED_TRANSFORMATION ( 'NONE', 'NONE', #7122,  #9440 ) ;
#3547 = ORIENTED_EDGE ( 'NONE', *, *, #10808, .F. ) ;
#3548 = CONICAL_SURFACE ( 'NONE', #11543, 5.000000000000000888, 1.047197551196600296 ) ;
#3549 = LINE ( 'NONE', #4740, #4279 ) ;
#3550 = ORIENTED_EDGE ( 'NONE', *, *, #10986, .F. ) ;
#3551 = ORIENTED_EDGE ( 'NONE', *, *, #2786, .F. ) ;
#3552 = CARTESIAN_POINT ( 'NONE',  ( 1.600000000000000089, 0.000000000000000000, 0.000000000000000000 ) ) ;
#3553 = CARTESIAN_POINT ( 'NONE',  ( -9.498873539028489220E-16, 10.00000000000000000, 210.0000000000000000 ) ) ;
#3554 = AXIS2_PLACEMENT_3D ( 'NONE', #4646, #5813, #1252 ) ;
#3555 = CARTESIAN_POINT ( 'NONE',  ( 6.466260427357672924, -2.904280683598006618, 5.030361703432631337 ) ) ;
#3556 = EDGE_CURVE ( 'NONE', #11091, #7485, #7993, .T. ) ;
#3557 = B_SPLINE_CURVE_WITH_KNOTS ( 'NONE', 3,
 ( #11801, #6130, #10634, #8401, #7301, #1701, #6205, #575 ),
 .UNSPECIFIED., .F., .F.,
 ( 4, 2, 2, 4 ),
 ( 2.459764730742321679E-07, 0.001920659145285711104, 0.002880865729692028403, 0.003841072314098346787 ),
 .UNSPECIFIED. ) ;
#3558 = AXIS2_PLACEMENT_3D ( 'NONE', #6429, #10928, #13211 ) ;
#3559 = CARTESIAN_POINT ( 'NONE',  ( 0.3572655899081595976, 2.309401076758508253, 3.999999999999993339 ) ) ;
#3560 = AXIS2_PLACEMENT_3D ( 'NONE', #7173, #584, #5393 ) ;
#3561 = UNCERTAINTY_MEASURE_WITH_UNIT (LENGTH_MEASURE( 1.000000000000000082E-05 ), #1076, 'distance_accuracy_value', 'NONE');
#3562 = DIRECTION ( 'NONE',  ( -0.000000000000000000, -0.000000000000000000, -1.000000000000000000 ) ) ;
#3563 = VERTEX_POINT ( 'NONE', #9977 ) ;
#3564 = AXIS2_PLACEMENT_3D ( 'NONE', #5747, #11485, #10244 ) ;
#3565 = STYLED_ITEM ( 'NONE', ( #12743 ), #6513 ) ;
#3566 = CARTESIAN_POINT ( 'NONE',  ( 229.2257385731837758, 308.4724102386206255, 182.7999999999996135 ) ) ;
#3567 = DIRECTION ( 'NONE',  ( 0.000000000000000000, 0.000000000000000000, 1.000000000000000000 ) ) ;
#3568 = DIRECTION ( 'NONE',  ( -1.000000000000000000, 0.000000000000000000, 0.000000000000000000 ) ) ;
#3569 = FACE_OUTER_BOUND ( 'NONE', #18, .T. ) ;
#3570 = ORIENTED_EDGE ( 'NONE', *, *, #12241, .F. ) ;
#3571 = ORIENTED_EDGE ( 'NONE', *, *, #14350, .T. ) ;
#3572 = CARTESIAN_POINT ( 'NONE',  ( 629.0024986820135382, 155.3908996001881064, 210.0000120000000265 ) ) ;
#3573 = FACE_OUTER_BOUND ( 'NONE', #6762, .T. ) ;
#3574 = VECTOR ( 'NONE', #12685, 1000.000000000000000 ) ;
#3575 = FACE_OUTER_BOUND ( 'NONE', #12948, .T. ) ;
#3576 = EDGE_CURVE ( 'NONE', #9582, #12254, #2819, .T. ) ;
#3577 = AXIS2_PLACEMENT_3D ( 'NONE', #12000, #1596, #7364 ) ;
#3578 = PRESENTATION_LAYER_ASSIGNMENT (  '', '', ( #1453 ) ) ;
#3579 = CYLINDRICAL_SURFACE ( 'NONE', #3803, 5.249999999999976907 ) ;
#3580 = ORIENTED_EDGE ( 'NONE', *, *, #9510, .T. ) ;
#3581 = AXIS2_PLACEMENT_3D ( 'NONE', #10518, #12883, #6018 ) ;
#3582 = VERTEX_POINT ( 'NONE', #14407 ) ;
#3583 = CARTESIAN_POINT ( 'NONE',  ( 0.000000000000000000, 0.000000000000000000, -210.0000000000000000 ) ) ;
#3584 = DIRECTION ( 'NONE',  ( 0.000000000000000000, 1.000000000000000000, -3.674212649225433764E-15 ) ) ;
#3585 = ADVANCED_FACE ( 'NONE', ( #59 ), #8936, .F. ) ;
#3586 = DIRECTION ( 'NONE',  ( 0.000000000000000000, 0.000000000000000000, -1.000000000000000000 ) ) ;
#3587 = CARTESIAN_POINT ( 'NONE',  ( 1.500000000000000444, 5.100000000000000533, 0.000000000000000000 ) ) ;
#3588 = FACE_OUTER_BOUND ( 'NONE', #6490, .T. ) ;
#3589 = FILL_AREA_STYLE ('',( #1128 ) ) ;
#3590 = APPLICATION_CONTEXT ( 'automotive_design' ) ;
#3591 = ORIENTED_EDGE ( 'NONE', *, *, #7451, .T. ) ;
#3592 = ADVANCED_FACE ( 'NONE', ( #9084 ), #2572, .T. ) ;
#3593 = MECHANICAL_DESIGN_GEOMETRIC_PRESENTATION_REPRESENTATION (  '', ( #11352 ), #11822 ) ;
#3594 = CARTESIAN_POINT ( 'NONE',  ( 635.0000000000000000, 160.0000000000000284, 187.5000000000000000 ) ) ;
#3595 = ORIENTED_EDGE ( 'NONE', *, *, #11330, .T. ) ;
#3596 = VERTEX_POINT ( 'NONE', #2213 ) ;
#3597 = B_SPLINE_CURVE_WITH_KNOTS ( 'NONE', 3,
 ( #1041, #10048, #11231, #10208, #3485 ),
 .UNSPECIFIED., .F., .F.,
 ( 4, 1, 4 ),
 ( 0.000000000000000000, 0.002886751345948130286, 0.005773502691896260572 ),
 .UNSPECIFIED. ) ;
#3598 = CARTESIAN_POINT ( 'NONE',  ( 459.3348797583643091, 272.6398425814014104, 210.0000000000000000 ) ) ;
#3599 = CONICAL_SURFACE ( 'NONE', #11825, 4.000000000000000000, 0.8911886515913786111 ) ;
#3600 = DIRECTION ( 'NONE',  ( -0.9578262852211514300, 0.2873478855663454401, 0.000000000000000000 ) ) ;
#3601 = CARTESIAN_POINT ( 'NONE',  ( 635.0000000000000000, 160.0000000000000284, 210.0000000000000000 ) ) ;
#3602 = AXIS2_PLACEMENT_3D ( 'NONE', #13219, #8495, #10713 ) ;
#3603 = ORIENTED_EDGE ( 'NONE', *, *, #4495, .T. ) ;
#3604 = DIRECTION ( 'NONE',  ( 0.000000000000000000, 0.000000000000000000, -1.000000000000000000 ) ) ;
#3605 = DIRECTION ( 'NONE',  ( 0.000000000000000000, 0.000000000000000000, -1.000000000000000000 ) ) ;
#3606 = EDGE_CURVE ( 'NONE', #2314, #10556, #3255, .T. ) ;
#3607 = DIRECTION ( 'NONE',  ( -0.000000000000000000, -0.000000000000000000, 1.000000000000000000 ) ) ;
#3608 = DIRECTION ( 'NONE',  ( 0.2873478855663497700, 0.9578262852211499867, 5.078292077360263497E-30 ) ) ;
#3609 = AXIS2_PLACEMENT_3D ( 'NONE', #14222, #9722, #6471 ) ;
#3610 = ORIENTED_EDGE ( 'NONE', *, *, #8996, .T. ) ;
#3611 = EDGE_CURVE ( 'NONE', #14241, #10194, #3189, .T. ) ;
#3612 = DIRECTION ( 'NONE',  ( 0.000000000000000000, 0.000000000000000000, -1.000000000000000000 ) ) ;
#3613 = ORIENTED_EDGE ( 'NONE', *, *, #859, .F. ) ;
#3614 = ORIENTED_EDGE ( 'NONE', *, *, #7142, .T. ) ;
#3615 = DIRECTION ( 'NONE',  ( -0.9237280213470676626, -0.3830490080632388272, 0.000000000000000000 ) ) ;
#3616 = CARTESIAN_POINT ( 'NONE',  ( 0.000000000000000000, 4.330127018922190985, -2.500000000000007105 ) ) ;
#3617 = FACE_OUTER_BOUND ( 'NONE', #5453, .T. ) ;
#3618 = ORIENTED_EDGE ( 'NONE', *, *, #1979, .T. ) ;
#3619 = CARTESIAN_POINT ( 'NONE',  ( 148.9991633467111569, 386.6211705227183870, 187.0000000000000568 ) ) ;
#3620 = LINE ( 'NONE', #9070, #9246 ) ;
#3621 = PLANE ( 'NONE',  #10386 ) ;
#3622 = CARTESIAN_POINT ( 'NONE',  ( 716.7018481736365629, 193.3416907550376322, 182.8000000000001535 ) ) ;
#3623 = EDGE_LOOP ( 'NONE', ( #2233, #10282, #12724, #12370 ) ) ;
#3624 = DIRECTION ( 'NONE',  ( 0.000000000000000000, 0.000000000000000000, -1.000000000000000000 ) ) ;
#3625 = CARTESIAN_POINT ( 'NONE',  ( 0.000000000000000000, 0.000000000000000000, -1.000000000000000000 ) ) ;
#3626 = CARTESIAN_POINT ( 'NONE',  ( 451.3035746174797396, 294.6698471414878782, 187.0000000000000568 ) ) ;
#3627 = ITEM_DEFINED_TRANSFORMATION ( 'NONE', 'NONE', #6430,  #9440 ) ;
#3628 = VERTEX_POINT ( 'NONE', #10039 ) ;
#3629 = CARTESIAN_POINT ( 'NONE',  ( 4.211140560182196957, 2.431303136016536470, -3.745885042887433514 ) ) ;
#3630 = ORIENTED_EDGE ( 'NONE', *, *, #426, .T. ) ;
#3631 = ORIENTED_EDGE ( 'NONE', *, *, #4308, .F. ) ;
#3632 = SURFACE_SIDE_STYLE ('',( #10263 ) ) ;
#3633 = CARTESIAN_POINT ( 'NONE',  ( 610.0000000000000000, 227.4403065089105951, -190.0000000000000000 ) ) ;
#3634 = B_SPLINE_CURVE_WITH_KNOTS ( 'NONE', 3,
 ( #6414, #9737, #924, #5447, #7436, #14455, #4125, #8615 ),
 .UNSPECIFIED., .F., .F.,
 ( 4, 2, 2, 4 ),
 ( 2.465131517071610173E-07, 0.001183067374689837636, 0.001774477805458902699, 0.002365888236227967761 ),
 .UNSPECIFIED. ) ;
#3635 = EDGE_CURVE ( 'NONE', #8892, #12461, #4301, .T. ) ;
#3636 = CARTESIAN_POINT ( 'NONE',  ( 6.518095160332178395, -2.933089652807374215, 5.080260301816945656 ) ) ;
#3637 = EDGE_CURVE ( 'NONE', #145, #7099, #11220, .T. ) ;
#3638 = DIRECTION ( 'NONE',  ( -0.2873478855663456066, -0.9578262852211514300, 7.452506120068652189E-15 ) ) ;
#3639 = DIRECTION ( 'NONE',  ( -0.000000000000000000, -0.000000000000000000, 1.000000000000000000 ) ) ;
#3640 = VERTEX_POINT ( 'NONE', #7690 ) ;
#3641 = CARTESIAN_POINT ( 'NONE',  ( -3.250000000000004441, 5.629165124598849879, 0.000000000000000000 ) ) ;
#3642 = DIRECTION ( 'NONE',  ( -1.000000000000000000, 0.000000000000000000, -0.000000000000000000 ) ) ;
#3643 = DIRECTION ( 'NONE',  ( 1.000000000000000000, 0.000000000000000000, 0.000000000000000000 ) ) ;
#3644 = CARTESIAN_POINT ( 'NONE',  ( -10.00000000000000000, 10.00000000000000178, -190.0000000000000000 ) ) ;
#3645 = EDGE_CURVE ( 'NONE', #2860, #4509, #3340, .T. ) ;
#3646 = EDGE_LOOP ( 'NONE', ( #11392, #4600, #8803, #8779, #10365, #1482 ) ) ;
#3647 = EDGE_LOOP ( 'NONE', ( #67, #14255, #1275 ) ) ;
#3648 = DIRECTION ( 'NONE',  ( 0.000000000000000000, 0.000000000000000000, 1.000000000000000000 ) ) ;
#3649 = FACE_OUTER_BOUND ( 'NONE', #55, .T. ) ;
#3650 = CARTESIAN_POINT ( 'NONE',  ( 6.506891779418573662, 2.833891091414751706, 5.091556646552823473 ) ) ;
#3651 = EDGE_LOOP ( 'NONE', ( #8860, #11368, #11150, #9833 ) ) ;
#3652 = AXIS2_PLACEMENT_3D ( 'NONE', #4425, #6712, #8923 ) ;
#3653 = ORIENTED_EDGE ( 'NONE', *, *, #2412, .T. ) ;
#3654 = DIRECTION ( 'NONE',  ( 0.000000000000000000, 0.000000000000000000, -1.000000000000000000 ) ) ;
#3655 = CARTESIAN_POINT ( 'NONE',  ( 145.1678582058265476, 408.6511750828048548, 190.0000000000000000 ) ) ;
#3656 = CARTESIAN_POINT ( 'NONE',  ( 6.420058897733093239, 5.782965130189193559, -4.012520129335570115E-16 ) ) ;
#3657 = DIRECTION ( 'NONE',  ( 1.000000000000000000, 9.498873539028489960E-17, 0.000000000000000000 ) ) ;
#3658 = DIRECTION ( 'NONE',  ( -0.000000000000000000, -0.000000000000000000, -1.000000000000000000 ) ) ;
#3659 = ADVANCED_FACE ( 'NONE', ( #881 ), #8865, .F. ) ;
#3660 = VERTEX_POINT ( 'NONE', #4521 ) ;
#3661 = CARTESIAN_POINT ( 'NONE',  ( -1.399999999999999689, 0.000000000000000000, 0.000000000000000000 ) ) ;
#3662 = ORIENTED_EDGE ( 'NONE', *, *, #6345, .F. ) ;
#3663 = ORIENTED_EDGE ( 'NONE', *, *, #11458, .F. ) ;
#3664 = CARTESIAN_POINT ( 'NONE',  ( 6.541333988313477121, -2.987057409892287740, -5.112749828287758369 ) ) ;
#3665 = DIRECTION ( 'NONE',  ( 0.000000000000000000, 0.000000000000000000, -1.000000000000000000 ) ) ;
#3666 = CARTESIAN_POINT ( 'NONE',  ( 610.0000000000001137, 191.1080398579018720, 190.0000000000000000 ) ) ;
#3667 = VERTEX_POINT ( 'NONE', #3476 ) ;
#3668 = DIRECTION ( 'NONE',  ( 0.9578262852211513190, -0.2873478855663453846, 0.000000000000000000 ) ) ;
#3669 = DIRECTION ( 'NONE',  ( 0.9578262852211507639, -0.2873478855663477716, 0.000000000000000000 ) ) ;
#3670 = CARTESIAN_POINT ( 'NONE',  ( 448.9584422793565750, 264.0194060144110608, 210.0000000000000000 ) ) ;
#3671 = LINE ( 'NONE', #3747, #3141 ) ;
#3672 = ADVANCED_FACE ( 'NONE', ( #5480 ), #12250, .F. ) ;
#3673 = ORIENTED_EDGE ( 'NONE', *, *, #13691, .F. ) ;
#3674 = CARTESIAN_POINT ( 'NONE',  ( 0.4465819873851997746, 2.886751345948125547, 4.999999999999999112 ) ) ;
#3675 = VERTEX_POINT ( 'NONE', #7971 ) ;
#3676 = ADVANCED_FACE ( 'NONE', ( #12392 ), #10198, .F. ) ;
#3677 = ORIENTED_EDGE ( 'NONE', *, *, #13247, .F. ) ;
#3678 = DIRECTION ( 'NONE',  ( -0.000000000000000000, 0.000000000000000000, 1.000000000000000000 ) ) ;
#3679 = EDGE_CURVE ( 'NONE', #5458, #6536, #10116, .T. ) ;
#3680 = EDGE_CURVE ( 'NONE', #3017, #14524, #1181, .T. ) ;
#3681 = CARTESIAN_POINT ( 'NONE',  ( -4.000000000000000000, -0.3979232138631226823, -3.896351557369779711E-17 ) ) ;
#3682 = DIRECTION ( 'NONE',  ( 0.000000000000000000, -1.000000000000000000, 0.000000000000000000 ) ) ;
#3683 = EDGE_CURVE ( 'NONE', #8233, #5419, #9901, .T. ) ;
#3684 = VERTEX_POINT ( 'NONE', #1033 ) ;
#3685 = CARTESIAN_POINT ( 'NONE',  ( 3.309651814758565180, -5.455921364805393026, -1.000000000000000000 ) ) ;
#3686 = EDGE_CURVE ( 'NONE', #13114, #8286, #4436, .T. ) ;
#3687 = FACE_OUTER_BOUND ( 'NONE', #8533, .T. ) ;
#3688 = DIRECTION ( 'NONE',  ( -1.000000000000000000, 0.000000000000000000, 0.000000000000000000 ) ) ;
#3689 = CARTESIAN_POINT ( 'NONE',  ( 2.500000000000000000, 1.178949249685212974, -2.042000000000001148 ) ) ;
#3690 = ORIENTED_EDGE ( 'NONE', *, *, #11875, .T. ) ;
#3691 = FACE_OUTER_BOUND ( 'NONE', #5407, .T. ) ;
#3692 = ADVANCED_BREP_SHAPE_REPRESENTATION ( '', ( #7462, #9440 ), #10411 ) ;
#3693 = CONTEXT_DEPENDENT_SHAPE_REPRESENTATION ( #6598, #13134 ) ;
#3694 = ORIENTED_EDGE ( 'NONE', *, *, #8562, .T. ) ;
#3695 = DIRECTION ( 'NONE',  ( -0.000000000000000000, 1.000000000000000000, -0.000000000000000000 ) ) ;
#3696 = ORIENTED_EDGE ( 'NONE', *, *, #5732, .T. ) ;
#3697 = ORIENTED_EDGE ( 'NONE', *, *, #493, .T. ) ;
#3698 = FILL_AREA_STYLE ('',( #13807 ) ) ;
#3699 = DIRECTION ( 'NONE',  ( -0.7071067811865364705, 0.000000000000000000, 0.7071067811865584529 ) ) ;
#3700 = EDGE_CURVE ( 'NONE', #9517, #3531, #280, .T. ) ;
#3701 = ADVANCED_FACE ( 'NONE', ( #13880 ), #12844, .F. ) ;
#3702 = CARTESIAN_POINT ( 'NONE',  ( -0.2500000000000000000, -8.096141056083446585, 0.000000000000000000 ) ) ;
#3703 = CARTESIAN_POINT ( 'NONE',  ( 4.555094537983153558, 5.243183837310242623, -6.208110906918258287 ) ) ;
#3704 = UNCERTAINTY_MEASURE_WITH_UNIT (LENGTH_MEASURE( 1.000000000000000082E-05 ), #3524, 'distance_accuracy_value', 'NONE');
#3705 = CARTESIAN_POINT ( 'NONE',  ( 0.4465819873852049926, -5.773502691896264416, 5.911082023588295771E-17 ) ) ;
#3706 = ORIENTED_EDGE ( 'NONE', *, *, #14406, .T. ) ;
#3707 = EDGE_CURVE ( 'NONE', #3419, #14577, #12692, .T. ) ;
#3708 = DIRECTION ( 'NONE',  ( -0.000000000000000000, 1.000000000000000000, 0.000000000000000000 ) ) ;
#3709 = PLANE ( 'NONE',  #11986 ) ;
#3710 = DIRECTION ( 'NONE',  ( 0.000000000000000000, 0.000000000000000000, 1.000000000000000000 ) ) ;
#3711 = EDGE_CURVE ( 'NONE', #5965, #12303, #8116, .T. ) ;
#3712 = CARTESIAN_POINT ( 'NONE',  ( 6.527192678185236296, 2.941622124011284978, 5.095038975456149366 ) ) ;
#3713 = CIRCLE ( 'NONE', #1818, 4.200000000000009059 ) ;
#3714 = ORIENTED_EDGE ( 'NONE', *, *, #829, .T. ) ;
#3715 = EDGE_LOOP ( 'NONE', ( #10104, #12863, #363, #4291 ) ) ;
#3716 = CARTESIAN_POINT ( 'NONE',  ( 642.5000000000001137, 160.0000000000000284, -222.5000000000000000 ) ) ;
#3717 = CYLINDRICAL_SURFACE ( 'NONE', #1885, 7.500000000000062172 ) ;
#3718 = CARTESIAN_POINT ( 'NONE',  ( 6.092449800118089343, 4.833012432206481357, 1.628976913806340798 ) ) ;
#3720 = EDGE_LOOP ( 'NONE', ( #9824, #9905, #9349, #884 ) ) ;
#3719 = AXIS2_PLACEMENT_3D ( 'NONE', #1322, #10322, #191 ) ;
#3721 = CIRCLE ( 'NONE', #14552, 2.396904916527699214 ) ;
#3722 = CARTESIAN_POINT ( 'NONE',  ( 0.000000000000000000, 0.000000000000000000, -187.0000000000000000 ) ) ;
#3723 = CARTESIAN_POINT ( 'NONE',  ( -6.259644161404860030E-16, -4.618802153517027165, -3.433295621305388234 ) ) ;
#3724 = CARTESIAN_POINT ( 'NONE',  ( -1.499999999999999556, 6.975000000000000533, 0.000000000000000000 ) ) ;
#3725 = B_SPLINE_CURVE_WITH_KNOTS ( 'NONE', 3,
 ( #3728, #9557, #3941, #13765, #8429, #6079, #8138, #12644, #4839, #12723 ),
 .UNSPECIFIED., .F., .F.,
 ( 4, 2, 2, 2, 4 ),
 ( 0.000000000000000000, 0.001989602278884364858, 0.003979204557768729715, 0.005968806836653094139, 0.007958409115537459430 ),
 .UNSPECIFIED. ) ;
#3726 = CARTESIAN_POINT ( 'NONE',  ( 635.0000000000000000, 235.0000000000000284, -263.5000000000000000 ) ) ;
#3727 = CARTESIAN_POINT ( 'NONE',  ( 639.0000000000000000, 156.0000000000000000, -233.5000000000000000 ) ) ;
#3728 = CARTESIAN_POINT ( 'NONE',  ( -6.837824896291514243, 3.947820044545427454, -6.564402953523716278 ) ) ;
#3729 =( NAMED_UNIT ( * ) SI_UNIT ( $, .STERADIAN. ) SOLID_ANGLE_UNIT ( ) );
#3730 = ORIENTED_EDGE ( 'NONE', *, *, #7451, .F. ) ;
#3731 = CARTESIAN_POINT ( 'NONE',  ( 615.0000000000000000, 160.0000000000000284, 187.5000000000000000 ) ) ;
#3732 = ORIENTED_EDGE ( 'NONE', *, *, #10575, .T. ) ;
#3733 = EDGE_LOOP ( 'NONE', ( #12839, #7716, #3860, #13532 ) ) ;
#3734 = CARTESIAN_POINT ( 'NONE',  ( 446.3084422793565409, 264.0194060144110608, 187.0000000000000000 ) ) ;
#3735 = PRESENTATION_LAYER_ASSIGNMENT (  '', '', ( #8188 ) ) ;
#3736 = PLANE ( 'NONE',  #10851 ) ;
#3737 = EDGE_CURVE ( 'NONE', #8153, #5571, #9884, .T. ) ;
#3738 = DIRECTION ( 'NONE',  ( 0.000000000000000000, 0.000000000000000000, 1.000000000000000000 ) ) ;
#3739 = CYLINDRICAL_SURFACE ( 'NONE', #13848, 2.100000000000000089 ) ;
#3740 = VERTEX_POINT ( 'NONE', #3702 ) ;
#3741 = DIRECTION ( 'NONE',  ( 0.9578262852211513190, -0.2873478855663455511, 1.110223024625158513E-15 ) ) ;
#3742 = CARTESIAN_POINT ( 'NONE',  ( 6.500000000000000000, -1.417018949932591365, -5.722407714414702085 ) ) ;
#3743 = CIRCLE ( 'NONE', #13633, 5.200000000000005507 ) ;
#3744 = VECTOR ( 'NONE', #1039, 1000.000000000000000 ) ;
#3745 = CIRCLE ( 'NONE', #2044, 4.199999999999981526 ) ;
#3746 = LINE ( 'NONE', #7273, #8893 ) ;
#3747 = CARTESIAN_POINT ( 'NONE',  ( -6.500000000000000000, -3.752776749732572803, -8.000000000000000000 ) ) ;
#3748 = ORIENTED_EDGE ( 'NONE', *, *, #3872, .F. ) ;
#3749 = CARTESIAN_POINT ( 'NONE',  ( 2.133938722758552675, 6.273523403446317204, -0.09463688534106567962 ) ) ;
#3750 = ORIENTED_EDGE ( 'NONE', *, *, #14606, .T. ) ;
#3751 = LINE ( 'NONE', #13563, #13168 ) ;
#3752 = VECTOR ( 'NONE', #7985, 1000.000000000000114 ) ;
#3753 = VECTOR ( 'NONE', #8043, 1000.000000000000114 ) ;
#3754 = CARTESIAN_POINT ( 'NONE',  ( 703.1581845006096501, 166.2926764603917036, 150.0000000000013927 ) ) ;
#3755 = EDGE_CURVE ( 'NONE', #4197, #5281, #11375, .T. ) ;
#3756 = FACE_OUTER_BOUND ( 'NONE', #10506, .T. ) ;
#3757 = ORIENTED_EDGE ( 'NONE', *, *, #141, .T. ) ;
#3758 = CARTESIAN_POINT ( 'NONE',  ( 610.0000000000001137, 191.1080398579019288, 190.0000000000000284 ) ) ;
#3759 = AXIS2_PLACEMENT_3D ( 'NONE', #2791, #12907, #7294 ) ;
#3760 = EDGE_CURVE ( 'NONE', #1120, #8086, #11584, .T. ) ;
#3761 = CYLINDRICAL_SURFACE ( 'NONE', #10195, 5.249999999999976907 ) ;
#3762 = DIRECTION ( 'NONE',  ( -1.148424442117023040E-15, 3.445273326351216045E-16, 1.000000000000000000 ) ) ;
#3763 = ORIENTED_EDGE ( 'NONE', *, *, #7837, .T. ) ;
#3764 = B_SPLINE_CURVE_WITH_KNOTS ( 'NONE', 3,
 ( #14311, #1763, #3102, #10766, #14179, #646, #14528, #11203, #5464, #6851, #12308, #11057, #1085, #938, #5675, #9881, #1017, #13420 ),
 .UNSPECIFIED., .F., .F.,
 ( 4, 2, 2, 2, 2, 2, 2, 2, 4 ),
 ( 0.5000000000000000000, 0.5625000000000000000, 0.6250000000000000000, 0.6875000000000000000, 0.7500000000000000000, 0.8125000000000000000, 0.8750000000000000000, 0.9375000000000000000, 1.000000000000000000 ),
 .UNSPECIFIED. ) ;
#3765 = AXIS2_PLACEMENT_3D ( 'NONE', #7403, #6282, #5184 ) ;
#3766 = EDGE_CURVE ( 'NONE', #8256, #3667, #5494, .T. ) ;
#3767 = CARTESIAN_POINT ( 'NONE',  ( -4.000000000000000000, 2.471528634177585282, -3.686887442155186712 ) ) ;
#3768 = DIRECTION ( 'NONE',  ( 0.000000000000000000, -1.000000000000000000, 0.000000000000000000 ) ) ;
#3769 = EDGE_LOOP ( 'NONE', ( #13617, #2536 ) ) ;
#3771 = EDGE_CURVE ( 'NONE', #9802, #7658, #9415, .T. ) ;
#3770 = FACE_OUTER_BOUND ( 'NONE', #10780, .T. ) ;
#3772 = VERTEX_POINT ( 'NONE', #6943 ) ;
#3773 = EDGE_LOOP ( 'NONE', ( #5069, #6788, #4171, #788 ) ) ;
#3774 = B_SPLINE_CURVE_WITH_KNOTS ( 'NONE', 3,
 ( #7546, #1935, #8802, #12175, #9978, #13523, #3703, #12624, #204, #9019 ),
 .UNSPECIFIED., .F., .F.,
 ( 4, 2, 2, 2, 4 ),
 ( 8.662740229329108052E-20, 0.001989602278884365725, 0.003979204557768730582, 0.005968806836653095874, 0.007958409115537461165 ),
 .UNSPECIFIED. ) ;
#3775 = LINE ( 'NONE', #199, #14158 ) ;
#3776 = VECTOR ( 'NONE', #9804, 1000.000000000000000 ) ;
#3777 = CARTESIAN_POINT ( 'NONE',  ( -9.999999999999980460, 413.4403065089106235, 190.0000000000000000 ) ) ;
#3778 = VECTOR ( 'NONE', #2260, 1000.000000000000000 ) ;
#3779 = CIRCLE ( 'NONE', #12009, 2.041999999999999815 ) ;
#3780 = DIRECTION ( 'NONE',  ( 0.000000000000000000, 0.000000000000000000, -1.000000000000000000 ) ) ;
#3781 = SHAPE_REPRESENTATION ( 'angular contact ball bearing_68_iso_ISO 15 ABB - 1710 - 20,SI,NC,20_68', ( #9440 ), #10888 ) ;
#3782 = VECTOR ( 'NONE', #11666, 1000.000000000000000 ) ;
#3783 = DIRECTION ( 'NONE',  ( -1.000000000000000000, 0.000000000000000000, 0.000000000000000000 ) ) ;
#3784 = VERTEX_POINT ( 'NONE', #7163 ) ;
#3785 = VECTOR ( 'NONE', #11447, 1000.000000000000000 ) ;
#3786 = EDGE_CURVE ( 'NONE', #14203, #5297, #538, .T. ) ;
#3787 = CARTESIAN_POINT ( 'NONE',  ( 629.0000000000000000, 166.0000000000000284, -187.5000000000000000 ) ) ;
#3788 = DIRECTION ( 'NONE',  ( -0.000000000000000000, -0.000000000000000000, 1.000000000000000000 ) ) ;
#3789 = DIRECTION ( 'NONE',  ( 0.000000000000000000, 0.000000000000000000, 1.000000000000000000 ) ) ;
#3790 = VECTOR ( 'NONE', #9846, 1000.000000000000000 ) ;
#3792 = EDGE_CURVE ( 'NONE', #10509, #4698, #11059, .T. ) ;
#3791 = CARTESIAN_POINT ( 'NONE',  ( 2.500000000000000000, 1.178949249685212974, -2.042000000000001148 ) ) ;
#3793 = AXIS2_PLACEMENT_3D ( 'NONE', #7219, #3762, #9585 ) ;
#3794 = EDGE_LOOP ( 'NONE', ( #3763, #2932, #585 ) ) ;
#3795 = EDGE_LOOP ( 'NONE', ( #257, #14445, #417, #4368 ) ) ;
#3796 = B_SPLINE_CURVE_WITH_KNOTS ( 'NONE', 3,
 ( #14041, #10712, #14257, #8637, #11882, #7310 ),
 .UNSPECIFIED., .F., .F.,
 ( 4, 2, 4 ),
 ( 0.002336974151641558160, 0.003500975885716449323, 0.004664977619791340485 ),
 .UNSPECIFIED. ) ;
#3797 = CARTESIAN_POINT ( 'NONE',  ( 8.500000000000000000, -2.886751345948120662, 4.999999999999999112 ) ) ;
#3798 = CARTESIAN_POINT ( 'NONE',  ( 0.000000000000000000, 2.357898499370431722, -2.818925648462311528E-15 ) ) ;
#3799 = CARTESIAN_POINT ( 'NONE',  ( -2.500000000000000888, 0.000000000000000000, -4.974599999999998801 ) ) ;
#3800 = AXIS2_PLACEMENT_3D ( 'NONE', #10548, #425, #4817 ) ;
#3801 = VECTOR ( 'NONE', #7457, 1000.000000000000000 ) ;
#3802 = DIRECTION ( 'NONE',  ( 0.000000000000000000, -0.000000000000000000, 1.000000000000000000 ) ) ;
#3803 = AXIS2_PLACEMENT_3D ( 'NONE', #8068, #4960, #2 ) ;
#3804 = ORIENTED_EDGE ( 'NONE', *, *, #3414, .T. ) ;
#3805 = CARTESIAN_POINT ( 'NONE',  ( 650.0000000000000000, 175.0000000000000568, -190.0000000000000000 ) ) ;
#3806 = CARTESIAN_POINT ( 'NONE',  ( 6.533910050139697390, -2.950514251728070469, -5.110440592449064567 ) ) ;
#3807 = CARTESIAN_POINT ( 'NONE',  ( 6.270061300899935297, -4.268872906156509828, -6.443866470201760954 ) ) ;
#3808 = CARTESIAN_POINT ( 'NONE',  ( 0.3572655899080433572, -2.309401076758680116, -4.000000000000000000 ) ) ;
#3809 = DIRECTION ( 'NONE',  ( 0.000000000000000000, 0.000000000000000000, 1.000000000000000000 ) ) ;
#3810 = SURFACE_STYLE_USAGE ( .BOTH. , #11831 ) ;
#3811 = AXIS2_PLACEMENT_3D ( 'NONE', #941, #14467, #8631 ) ;
#3812 = ORIENTED_EDGE ( 'NONE', *, *, #7191, .F. ) ;
#3813 = VECTOR ( 'NONE', #5439, 1000.000000000000000 ) ;
#3814 = PLANE ( 'NONE',  #1658 ) ;
#3815 = VERTEX_POINT ( 'NONE', #5764 ) ;
#3816 = ORIENTED_EDGE ( 'NONE', *, *, #12956, .F. ) ;
#3817 = DIRECTION ( 'NONE',  ( -1.000000000000000000, -0.000000000000000000, -0.000000000000000000 ) ) ;
#3818 = AXIS2_PLACEMENT_3D ( 'NONE', #6831, #11625, #13775 ) ;
#3819 = DIRECTION ( 'NONE',  ( 1.000000000000000000, 0.000000000000000000, -0.000000000000000000 ) ) ;
#3820 = VECTOR ( 'NONE', #6709, 1000.000000000000227 ) ;
#3821 = VECTOR ( 'NONE', #980, 1000.000000000000000 ) ;
#3822 = FACE_OUTER_BOUND ( 'NONE', #6084, .T. ) ;
#3823 = DIRECTION ( 'NONE',  ( 0.9578262852211508749, -0.2873478855663470499, 0.000000000000000000 ) ) ;
#3824 = ORIENTED_EDGE ( 'NONE', *, *, #14325, .F. ) ;
#3825 = LINE ( 'NONE', #11761, #256 ) ;
#3826 = DIRECTION ( 'NONE',  ( 0.000000000000000000, 0.000000000000000000, 1.000000000000000000 ) ) ;
#3827 = CARTESIAN_POINT ( 'NONE',  ( 6.534838248920900483, -5.903531555104837736, 5.201568163584232486E-16 ) ) ;
#3828 = CARTESIAN_POINT ( 'NONE',  ( 611.4942090049449916, 232.4210031920597999, 184.7999999999999829 ) ) ;
#3829 = ORIENTED_EDGE ( 'NONE', *, *, #3158, .F. ) ;
#3830 = CARTESIAN_POINT ( 'NONE',  ( 0.5204879950541921874, 7.205049615410631603, -0.5609245978742269934 ) ) ;
#3831 = ORIENTED_EDGE ( 'NONE', *, *, #10608, .T. ) ;
#3832 = VECTOR ( 'NONE', #6698, 1000.000000000000000 ) ;
#3833 = EDGE_CURVE ( 'NONE', #4638, #7367, #12554, .T. ) ;
#3834 = EDGE_CURVE ( 'NONE', #12569, #6919, #2306, .T. ) ;
#3835 = CARTESIAN_POINT ( 'NONE',  ( -9.137956343300853490, 374.5525593289319204, -184.8000000000000398 ) ) ;
#3836 = PRESENTATION_LAYER_ASSIGNMENT (  '', '', ( #14429 ) ) ;
#3837 = CARTESIAN_POINT ( 'NONE',  ( 610.8620436566990293, 230.3137853645732491, 184.7999999999999829 ) ) ;
#3838 = DIRECTION ( 'NONE',  ( -0.9578262852211498757, 0.2873478855663503251, -1.198990317802636355E-15 ) ) ;
#3839 = EDGE_LOOP ( 'NONE', ( #10057, #7560, #8717 ) ) ;
#3840 = CARTESIAN_POINT ( 'NONE',  ( -5.686050877451574337, -5.768780236673276995, -1.000000000000000000 ) ) ;
#3841 = CARTESIAN_POINT ( 'NONE',  ( 4.999999999999997335, 0.000000000000000000, 0.000000000000000000 ) ) ;
#3842 = CARTESIAN_POINT ( 'NONE',  ( 0.08165819712376755357, -3.720292241887083851, 3.556264818047238929 ) ) ;
#3843 = CARTESIAN_POINT ( 'NONE',  ( -5.357619327558935599E-16, 7.505553499465137612, -6.177802698399959880 ) ) ;
#3844 = ORIENTED_EDGE ( 'NONE', *, *, #647, .F. ) ;
#3845 = PRODUCT_DEFINITION_FORMATION_WITH_SPECIFIED_SOURCE ( 'ANY', '', #8160, .NOT_KNOWN. ) ;
#3846 = CARTESIAN_POINT ( 'NONE',  ( -3.999999999998910649, -1.658469974638591804, -3.531532913075256186 ) ) ;
#3847 = VERTEX_POINT ( 'NONE', #14249 ) ;
#3848 = EDGE_CURVE ( 'NONE', #9351, #13246, #9532, .T. ) ;
#3849 = FACE_OUTER_BOUND ( 'NONE', #3647, .T. ) ;
#3850 = ORIENTED_EDGE ( 'NONE', *, *, #14304, .F. ) ;
#3851 = VERTEX_POINT ( 'NONE', #9673 ) ;
#3852 = AXIS2_PLACEMENT_3D ( 'NONE', #9203, #5800, #5583 ) ;
#3853 = CIRCLE ( 'NONE', #5726, 5.200000000000004619 ) ;
#3854 = CARTESIAN_POINT ( 'NONE',  ( 2.344047193898588954, 3.265465875126468021, -5.031375706690542042E-16 ) ) ;
#3855 = CARTESIAN_POINT ( 'NONE',  ( -2.000000000000006661, 3.464101615137750834, 0.000000000000000000 ) ) ;
#3856 = EDGE_CURVE ( 'NONE', #5068, #12967, #1155, .T. ) ;
#3857 = CARTESIAN_POINT ( 'NONE',  ( -10.00000000000000000, 10.00000000000000178, 190.0000000000000000 ) ) ;
#3858 = VECTOR ( 'NONE', #2832, 1000.000000000000000 ) ;
#3859 = CARTESIAN_POINT ( 'NONE',  ( 628.0000000000000000, 235.0000000000000284, -233.5000000000000000 ) ) ;
#3860 = ORIENTED_EDGE ( 'NONE', *, *, #11979, .F. ) ;
#3861 = AXIS2_PLACEMENT_3D ( 'NONE', #2910, #13903, #7327 ) ;
#3862 = DIRECTION ( 'NONE',  ( 0.000000000000000000, 0.000000000000000000, 1.000000000000000000 ) ) ;
#3863 = LINE ( 'NONE', #8272, #3030 ) ;
#3864 = CARTESIAN_POINT ( 'NONE',  ( 635.0000000000000000, 160.0000000000000284, -208.5000000000000000 ) ) ;
#3865 = ADVANCED_FACE ( 'NONE', ( #9592 ), #3023, .T. ) ;
#3866 = DIRECTION ( 'NONE',  ( 0.000000000000000000, 0.000000000000000000, -1.000000000000000000 ) ) ;
#3867 = ORIENTED_EDGE ( 'NONE', *, *, #9171, .F. ) ;
#3868 = ORIENTED_EDGE ( 'NONE', *, *, #9803, .F. ) ;
#3869 = CARTESIAN_POINT ( 'NONE',  ( 4.000000000000000000, 2.309401076758497151, -3.433295621305379353 ) ) ;
#3870 = DIRECTION ( 'NONE',  ( -0.000000000000000000, -0.000000000000000000, -1.000000000000000000 ) ) ;
#3871 = DIRECTION ( 'NONE',  ( 1.000000000000000000, 0.000000000000000000, -0.000000000000000000 ) ) ;
#3872 = EDGE_CURVE ( 'NONE', #7124, #12661, #14031, .T. ) ;
#3873 = EDGE_CURVE ( 'NONE', #3847, #6036, #5167, .T. ) ;
#3874 = DIRECTION ( 'NONE',  ( -0.8571673013836776933, 0.000000000000000000, -0.5150380737757388472 ) ) ;
#3875 = EDGE_LOOP ( 'NONE', ( #9687, #10191 ) ) ;
#3876 = EDGE_CURVE ( 'NONE', #3508, #4822, #10702, .T. ) ;
#3877 = DIRECTION ( 'NONE',  ( -0.000000000000000000, -0.000000000000000000, -1.000000000000000000 ) ) ;
#3878 = LINE ( 'NONE', #300, #10656 ) ;
#3879 = CARTESIAN_POINT ( 'NONE',  ( 6.367873360227558344, -2.886751345948134873, -5.000000000000000000 ) ) ;
#3880 = CARTESIAN_POINT ( 'NONE',  ( 142.4540310085880606, 355.9707293956415697, -187.0000000000000000 ) ) ;
#3881 = CARTESIAN_POINT ( 'NONE',  ( 2.500000000000000000, -2.357898499370432166, 3.035766082959412415E-15 ) ) ;
#3882 = FILL_AREA_STYLE_COLOUR ( '', #3151 ) ;
#3883 =( LENGTH_UNIT ( ) NAMED_UNIT ( * ) SI_UNIT ( .MILLI., .METRE. ) );
#3884 = ORIENTED_EDGE ( 'NONE', *, *, #4475, .F. ) ;
#3885 = CARTESIAN_POINT ( 'NONE',  ( 3.522875095019493141, -2.820352903225631369, -3.598441714920572299 ) ) ;
#3886 = ORIENTED_EDGE ( 'NONE', *, *, #5739, .F. ) ;
#3887 = ORIENTED_EDGE ( 'NONE', *, *, #1315, .F. ) ;
#3888 = CARTESIAN_POINT ( 'NONE',  ( 455.5035746174796714, 294.6698471414878782, -190.0000000000000568 ) ) ;
#3889 = FACE_OUTER_BOUND ( 'NONE', #6270, .T. ) ;
#3890 = DIRECTION ( 'NONE',  ( 0.000000000000000000, 0.000000000000000000, -1.000000000000000000 ) ) ;
#3891 = CARTESIAN_POINT ( 'NONE',  ( 7.240873133980807452, 470.9098836221799047, -190.0000000000001990 ) ) ;
#3892 = EDGE_LOOP ( 'NONE', ( #11616, #5955, #4440, #10151, #4414, #10675, #8349, #5616, #3915, #10949, #3663, #10239, #8668, #1673, #12573, #3128 ) ) ;
#3893 = CARTESIAN_POINT ( 'NONE',  ( 459.7035746174795463, 294.6698471414878782, -210.0000000000000000 ) ) ;
#3894 = DIRECTION ( 'NONE',  ( -0.000000000000000000, -0.000000000000000000, -1.000000000000000000 ) ) ;
#3895 = PLANE ( 'NONE',  #10767 ) ;
#3896 = SURFACE_SIDE_STYLE ('',( #1742 ) ) ;
#3897 = ORIENTED_EDGE ( 'NONE', *, *, #6283, .T. ) ;
#3898 = ADVANCED_FACE ( 'NONE', ( #10925 ), #7447, .F. ) ;
#3899 = CARTESIAN_POINT ( 'NONE',  ( 0.1739375980333716654, 3.358985280702821097, 4.182066831946702479 ) ) ;
#3900 = CARTESIAN_POINT ( 'NONE',  ( 6.436591462021373999, 2.894509378375945019, -5.013437306331756105 ) ) ;
#3901 = ORIENTED_EDGE ( 'NONE', *, *, #5499, .F. ) ;
#3902 = EDGE_CURVE ( 'NONE', #2593, #7285, #14096, .T. ) ;
#3903 = B_SPLINE_CURVE_WITH_KNOTS ( 'NONE', 3,
 ( #4284, #13282, #3393, #3173, #3234, #7676, #2042, #2117, #4722, #5809, #11420, #1244, #9130, #10394, #11484, #1379, #103, #8028 ),
 .UNSPECIFIED., .F., .F.,
 ( 4, 2, 2, 2, 2, 2, 2, 2, 4 ),
 ( 0.000000000000000000, 0.06250000000000000000, 0.1250000000000000000, 0.1875000000000000000, 0.2500000000000000000, 0.3125000000000000000, 0.3750000000000000000, 0.4375000000000000000, 0.5000000000000000000 ),
 .UNSPECIFIED. ) ;
#3904 = FACE_BOUND ( 'NONE', #7831, .T. ) ;
#3905 = CARTESIAN_POINT ( 'NONE',  ( 6.815830331203685866, 1.228021141713631082E-13, -6.171384342982610960 ) ) ;
#3906 = CARTESIAN_POINT ( 'NONE',  ( 615.0000000000000000, 160.0000000000000284, -187.5000000000000000 ) ) ;
#3907 = ADVANCED_BREP_SHAPE_REPRESENTATION ( '', ( #11938, #9440 ), #7553 ) ;
#3908 = EDGE_LOOP ( 'NONE', ( #9919, #6980, #10427, #10740 ) ) ;
#3909 = DIRECTION ( 'NONE',  ( 0.000000000000000000, -1.000000000000000000, 0.000000000000000000 ) ) ;
#3910 = DIRECTION ( 'NONE',  ( 0.000000000000000000, 0.000000000000000000, 1.000000000000000000 ) ) ;
#3911 = LINE ( 'NONE', #9664, #13924 ) ;
#3912 = ORIENTED_EDGE ( 'NONE', *, *, #13781, .T. ) ;
#3913 = ORIENTED_EDGE ( 'NONE', *, *, #2775, .T. ) ;
#3914 = DIRECTION ( 'NONE',  ( 0.000000000000000000, 0.000000000000000000, -1.000000000000000000 ) ) ;
#3915 = ORIENTED_EDGE ( 'NONE', *, *, #3135, .F. ) ;
#3916 = CARTESIAN_POINT ( 'NONE',  ( 6.663127973346360200, -3.846958729056453308, -6.460793508093580328 ) ) ;
#3917 = PLANE ( 'NONE',  #11757 ) ;
#3918 = CARTESIAN_POINT ( 'NONE',  ( 636.7717819724297215, 155.3244477714206653, 210.0000000000000000 ) ) ;
#3919 = ADVANCED_FACE ( 'NONE', ( #1830, #5315, #727 ), #3917, .F. ) ;
#3920 = ADVANCED_FACE ( 'NONE', ( #1618, #7521, #3987 ), #12915, .F. ) ;
#3921 = CARTESIAN_POINT ( 'NONE',  ( -9.498873539028489220E-16, 10.00000000000000000, 190.0000000000000000 ) ) ;
#3922 = DIRECTION ( 'NONE',  ( -0.000000000000000000, -0.000000000000000000, 1.000000000000000000 ) ) ;
#3923 = ORIENTED_EDGE ( 'NONE', *, *, #7567, .T. ) ;
#3924 = DIRECTION ( 'NONE',  ( -0.2873478855663894049, -0.9578262852211382183, 0.000000000000000000 ) ) ;
#3925 = CARTESIAN_POINT ( 'NONE',  ( -0.6448876103708541807, -4.246476118072358474, -0.2256878752776773356 ) ) ;
#3926 = SHAPE_DEFINITION_REPRESENTATION ( #2259, #2822 ) ;
#3927 = CARTESIAN_POINT ( 'NONE',  ( 6.534533895392294234, 2.951347675328725106, 5.111884124469659341 ) ) ;
#3928 = ORIENTED_EDGE ( 'NONE', *, *, #12978, .F. ) ;
#3929 = ORIENTED_EDGE ( 'NONE', *, *, #5456, .F. ) ;
#3930 = CARTESIAN_POINT ( 'NONE',  ( 703.1581845006096501, 166.2926764603917036, 177.6000000000001648 ) ) ;
#3931 = CARTESIAN_POINT ( 'NONE',  ( -4.000000000000000000, 2.309401076758498483, -5.000000000000000000 ) ) ;
#3932 = CARTESIAN_POINT ( 'NONE',  ( -1.083333333333333037, -6.880090707843053544, -5.848636054922041083 ) ) ;
#3933 = EDGE_CURVE ( 'NONE', #8797, #12920, #3557, .T. ) ;
#3934 = ORIENTED_EDGE ( 'NONE', *, *, #4412, .F. ) ;
#3935 = CYLINDRICAL_SURFACE ( 'NONE', #4310, 2.199999999999984635 ) ;
#3936 = CARTESIAN_POINT ( 'NONE',  ( 6.367873360227558344, -2.886751345948134873, -5.000000000000000000 ) ) ;
#3937 = DIRECTION ( 'NONE',  ( 0.000000000000000000, 0.000000000000000000, -1.000000000000000000 ) ) ;
#3938 = ADVANCED_FACE ( 'NONE', ( #5099 ), #8482, .F. ) ;
#3939 = CARTESIAN_POINT ( 'NONE',  ( 1.499999999999999778, 7.399999999999999467, 0.000000000000000000 ) ) ;
#3940 = FACE_OUTER_BOUND ( 'NONE', #11238, .T. ) ;
#3941 = CARTESIAN_POINT ( 'NONE',  ( -5.698650001973517121, 4.592339236403562452, -6.344532336093705815 ) ) ;
#3942 = ORIENTED_EDGE ( 'NONE', *, *, #8104, .T. ) ;
#3943 = EDGE_CURVE ( 'NONE', #689, #8255, #3529, .T. ) ;
#3944 = CARTESIAN_POINT ( 'NONE',  ( -4.211140560182196957, 2.431303136016537803, -3.745885042887433514 ) ) ;
#3945 = ORIENTED_EDGE ( 'NONE', *, *, #9548, .F. ) ;
#3946 = ORIENTED_EDGE ( 'NONE', *, *, #12408, .T. ) ;
#3947 = CARTESIAN_POINT ( 'NONE',  ( 0.000000000000000000, 0.000000000000000000, 2.500000000000000444 ) ) ;
#3948 = ADVANCED_FACE ( 'NONE', ( #2198, #4417, #13344 ), #6562, .F. ) ;
#3949 = AXIS2_PLACEMENT_3D ( 'NONE', #1169, #1091, #4511 ) ;
#3950 = DIRECTION ( 'NONE',  ( -0.9237280213470676626, -0.3830490080632388272, 0.000000000000000000 ) ) ;
#3951 = AXIS2_PLACEMENT_3D ( 'NONE', #1147, #3522, #6913 ) ;
#3952 = DIRECTION ( 'NONE',  ( 1.000000000000000000, 0.000000000000000000, 0.000000000000000000 ) ) ;
#3953 = CARTESIAN_POINT ( 'NONE',  ( 1.083333333333333703, 6.880090707843044662, -5.848636054922036642 ) ) ;
#3954 = ORIENTED_EDGE ( 'NONE', *, *, #7804, .F. ) ;
#3955 = DIRECTION ( 'NONE',  ( 0.000000000000000000, -5.337610695313242707E-15, 1.000000000000000000 ) ) ;
#3956 = CARTESIAN_POINT ( 'NONE',  ( -8.074769166705394241, 378.0965165842501392, -187.0000000000000000 ) ) ;
#3957 = DIRECTION ( 'NONE',  ( 0.000000000000000000, 0.000000000000000000, 1.000000000000000000 ) ) ;
#3958 = DIRECTION ( 'NONE',  ( -0.000000000000000000, -0.000000000000000000, 1.000000000000000000 ) ) ;
#3959 = VERTEX_POINT ( 'NONE', #12158 ) ;
#3960 = EDGE_CURVE ( 'NONE', #3137, #1936, #8915, .T. ) ;
#3961 = CIRCLE ( 'NONE', #11019, 4.199999999999926459 ) ;
#3962 = ADVANCED_FACE ( 'NONE', ( #4498 ), #4574, .T. ) ;
#3963 = DIRECTION ( 'NONE',  ( 1.000000000000000000, 0.000000000000000000, 0.000000000000000000 ) ) ;
#3964 = CARTESIAN_POINT ( 'NONE',  ( 470.8287951810180516, 310.9528939902474463, -210.0000000000000000 ) ) ;
#3965 = ITEM_DEFINED_TRANSFORMATION ( 'NONE', 'NONE', #3364,  #9440 ) ;
#3966 = VECTOR ( 'NONE', #11180, 1000.000000000000000 ) ;
#3967 = EDGE_LOOP ( 'NONE', ( #7443, #11520, #6970, #12506 ) ) ;
#3968 = EDGE_CURVE ( 'NONE', #13396, #7052, #5879, .T. ) ;
#3969 = DIRECTION ( 'NONE',  ( 1.000000000000000000, 0.000000000000000000, 0.000000000000000000 ) ) ;
#3970 = CARTESIAN_POINT ( 'NONE',  ( -6.500000000000000000, 3.752776749732564809, -6.064240316920399110 ) ) ;
#3971 = CARTESIAN_POINT ( 'NONE',  ( -8.505790995054773873, 418.4210031920615620, -187.0000000000000000 ) ) ;
#3972 = AXIS2_PLACEMENT_3D ( 'NONE', #14193, #11819, #8350 ) ;
#3973 = AXIS2_PLACEMENT_3D ( 'NONE', #14419, #4311, #8870 ) ;
#3974 = ORIENTED_EDGE ( 'NONE', *, *, #6287, .T. ) ;
#3975 = CARTESIAN_POINT ( 'NONE',  ( 610.4437618601435815, 188.9679398019578116, 185.9079617568160074 ) ) ;
#3976 = CARTESIAN_POINT ( 'NONE',  ( 631.0000000000000000, 155.9999999999999432, -225.5000000000000000 ) ) ;
#3977 = LINE ( 'NONE', #412, #8975 ) ;
#3978 = DIRECTION ( 'NONE',  ( 0.000000000000000000, 0.000000000000000000, 1.000000000000000000 ) ) ;
#3979 = ORIENTED_EDGE ( 'NONE', *, *, #13006, .T. ) ;
#3980 = LINE ( 'NONE', #12088, #10777 ) ;
#3981 = ORIENTED_EDGE ( 'NONE', *, *, #5742, .F. ) ;
#3982 = ORIENTED_EDGE ( 'NONE', *, *, #11875, .F. ) ;
#3983 = AXIS2_PLACEMENT_3D ( 'NONE', #13343, #4416, #13417 ) ;
#3984 = CIRCLE ( 'NONE', #4696, 2.649999999999985700 ) ;
#3985 = ORIENTED_EDGE ( 'NONE', *, *, #10710, .F. ) ;
#3986 = LINE ( 'NONE', #7228, #6326 ) ;
#3987 = FACE_OUTER_BOUND ( 'NONE', #13183, .T. ) ;
#3988 = AXIS2_PLACEMENT_3D ( 'NONE', #10730, #3131, #756 ) ;
#3989 = CARTESIAN_POINT ( 'NONE',  ( 6.541334219041336162, 2.934241909852038699, -5.143243597038031467 ) ) ;
#3990 = LINE ( 'NONE', #3857, #14392 ) ;
#3991 = CONICAL_SURFACE ( 'NONE', #6108, 4.000000000000000000, 0.8911886515913786111 ) ;
#3992 = AXIS2_PLACEMENT_3D ( 'NONE', #6474, #838, #14229 ) ;
#3993 = UNCERTAINTY_MEASURE_WITH_UNIT (LENGTH_MEASURE( 1.000000000000000082E-05 ), #2035, 'distance_accuracy_value', 'NONE');
#3994 = CARTESIAN_POINT ( 'NONE',  ( 636.9746078850427011, 155.6249658629529620, 211.0000000000000000 ) ) ;
#3995 = ORIENTED_EDGE ( 'NONE', *, *, #518, .F. ) ;
#3996 = DIRECTION ( 'NONE',  ( 1.000000000000000000, 0.000000000000000000, 0.000000000000000000 ) ) ;
#3997 = DIRECTION ( 'NONE',  ( 1.000000000000000000, 0.000000000000000000, -0.000000000000000000 ) ) ;
#3998 = APPLICATION_PROTOCOL_DEFINITION ( 'draft international standard', 'automotive_design', 1998, #3590 ) ;
#3999=STYLED_ITEM('',(#14688),#7422);
#4000 = DIRECTION ( 'NONE',  ( -0.9237280213470676626, -0.3830490080632388272, 0.000000000000000000 ) ) ;
#4001 = ORIENTED_EDGE ( 'NONE', *, *, #12847, .T. ) ;
#4002 = VERTEX_POINT ( 'NONE', #8997 ) ;
#4003 = DIRECTION ( 'NONE',  ( -1.000000000000000000, 0.000000000000000000, 0.000000000000000000 ) ) ;
#4004 = CARTESIAN_POINT ( 'NONE',  ( 440.1783540539412343, 278.3868002927283101, -210.0000000000000000 ) ) ;
#4005 = EDGE_CURVE ( 'NONE', #5821, #11723, #11054, .T. ) ;
#4006 = VECTOR ( 'NONE', #4070, 1000.000000000000000 ) ;
#4007 = CIRCLE ( 'NONE', #9886, 5.750000000000000000 ) ;
#4008 = EDGE_CURVE ( 'NONE', #5188, #7721, #5888, .T. ) ;
#4009 = LINE ( 'NONE', #8419, #8472 ) ;
#4010 = CARTESIAN_POINT ( 'NONE',  ( 635.0000000000000000, 160.0000000000000284, -222.5000000000000000 ) ) ;
#4011 = VECTOR ( 'NONE', #6688, 1000.000000000000000 ) ;
#4012 = VERTEX_POINT ( 'NONE', #5463 ) ;
#4013 = FACE_BOUND ( 'NONE', #14383, .T. ) ;
#4014 = CARTESIAN_POINT ( 'NONE',  ( 1.098735407079667992, 7.248058225760153128, -6.326622577870739228 ) ) ;
#4015 = DIRECTION ( 'NONE',  ( 1.000000000000000000, 0.000000000000000000, 0.000000000000000000 ) ) ;
#4016 = VECTOR ( 'NONE', #2029, 1000.000000000000227 ) ;
#4017 = AXIS2_PLACEMENT_3D ( 'NONE', #4689, #367, #3584 ) ;
#4018 = LINE ( 'NONE', #14055, #885 ) ;
#4019 = CARTESIAN_POINT ( 'NONE',  ( 707.5067158355135462, 173.1315561368708700, 150.0000000000013642 ) ) ;
#4020 = DIRECTION ( 'NONE',  ( -0.2873478855663454401, -0.9578262852211514300, 0.000000000000000000 ) ) ;
#4021 = ORIENTED_EDGE ( 'NONE', *, *, #4371, .F. ) ;
#4022 = FACE_OUTER_BOUND ( 'NONE', #13986, .T. ) ;
#4023 = VERTEX_POINT ( 'NONE', #9961 ) ;
#4024 = ORIENTED_EDGE ( 'NONE', *, *, #8205, .F. ) ;
#4025 = AXIS2_PLACEMENT_3D ( 'NONE', #8257, #10482, #2663 ) ;
#4026 = FACE_OUTER_BOUND ( 'NONE', #9763, .T. ) ;
#4027 = ADVANCED_FACE ( 'NONE', ( #1016 ), #5526, .T. ) ;
#4028 = CIRCLE ( 'NONE', #5907, 4.799999999999999822 ) ;
#4029 = AXIS2_PLACEMENT_3D ( 'NONE', #9520, #8552, #13864 ) ;
#4030 = CARTESIAN_POINT ( 'NONE',  ( -1.500000000000001332, 0.000000000000000000, -6.975000000000000533 ) ) ;
#4031 = CARTESIAN_POINT ( 'NONE',  ( -0.1920286436967153787, 0.000000000000000000, 0.000000000000000000 ) ) ;
#4033 = ADVANCED_FACE ( 'NONE', ( #1084 ), #13208, .T. ) ;
#4032 = PLANE ( 'NONE',  #8421 ) ;
#4034 = VECTOR ( 'NONE', #6135, 1000.000000000000000 ) ;
#4035 = ORIENTED_EDGE ( 'NONE', *, *, #9352, .F. ) ;
#4036 = CARTESIAN_POINT ( 'NONE',  ( 153.1991633467111456, 386.6211705227183870, 190.0000000000000568 ) ) ;
#4037 = CARTESIAN_POINT ( 'NONE',  ( 6.500000000000000888, 4.077976443323007238, -6.122137821720842865 ) ) ;
#4038 = VECTOR ( 'NONE', #3157, 1000.000000000000000 ) ;
#4039 = CARTESIAN_POINT ( 'NONE',  ( 0.000000000000000000, 0.000000000000000000, -6.800000000000000711 ) ) ;
#4040 = FILL_AREA_STYLE_COLOUR ( '', #9735 ) ;
#4041 = ORIENTED_EDGE ( 'NONE', *, *, #13021, .F. ) ;
#4042 = VECTOR ( 'NONE', #8819, 1000.000000000000000 ) ;
#4043 = DIRECTION ( 'NONE',  ( 0.000000000000000000, 0.000000000000000000, -1.000000000000000000 ) ) ;
#4044 = CARTESIAN_POINT ( 'NONE',  ( 2.999999999999999112, -2.309401076758485605, 3.999999999999999112 ) ) ;
#4045 = ITEM_DEFINED_TRANSFORMATION ( 'NONE', 'NONE', #8066,  #9440 ) ;
#4046 = VERTEX_POINT ( 'NONE', #13500 ) ;
#4047 = EDGE_CURVE ( 'NONE', #1071, #8142, #12377, .T. ) ;
#4049 = CARTESIAN_POINT ( 'NONE',  ( 4.000000000000000000, -2.309401076758514915, -3.433295621305383349 ) ) ;
#4048 = AXIS2_PLACEMENT_3D ( 'NONE', #5748, #8033, #12536 ) ;
#4050 = AXIS2_PLACEMENT_3D ( 'NONE', #4108, #827, #8594 ) ;
#4051 = LINE ( 'NONE', #11918, #13669 ) ;
#4053 = CARTESIAN_POINT ( 'NONE',  ( -0.5000000000000000000, -6.429618962271402616, -1.000000000000000000 ) ) ;
#4052 = VECTOR ( 'NONE', #4785, 1000.000000000000227 ) ;
#4054 = EDGE_CURVE ( 'NONE', #12397, #6727, #7540, .T. ) ;
#4055 = EDGE_LOOP ( 'NONE', ( #7175, #3824, #2794, #10685 ) ) ;
#4056 = FACE_OUTER_BOUND ( 'NONE', #12606, .T. ) ;
#4057 = DIRECTION ( 'NONE',  ( 0.000000000000000000, 0.000000000000000000, -1.000000000000000000 ) ) ;
#4058 = EDGE_CURVE ( 'NONE', #5634, #13901, #6641, .T. ) ;
#4059 = PRODUCT_DEFINITION ( 'UNKNOWN', '', #5954, #13137 ) ;
#4060 = LINE ( 'NONE', #3976, #14199 ) ;
#4061 = CARTESIAN_POINT ( 'NONE',  ( 6.500000000000000000, 3.453380256388213887, -0.6809028088495826525 ) ) ;
#4062 = AXIS2_PLACEMENT_3D ( 'NONE', #13779, #4922, #3668 ) ;
#4063 = ORIENTED_EDGE ( 'NONE', *, *, #12359, .T. ) ;
#4064 =( NAMED_UNIT ( * ) SI_UNIT ( $, .STERADIAN. ) SOLID_ANGLE_UNIT ( ) );
#4065 = ORIENTED_EDGE ( 'NONE', *, *, #8983, .T. ) ;
#4066 = APPLICATION_CONTEXT ( 'automotive_design' ) ;
#4067 = ADVANCED_BREP_SHAPE_REPRESENTATION ( '', ( #7073, #9440 ), #7588 ) ;
#4068 = ORIENTED_EDGE ( 'NONE', *, *, #10181, .F. ) ;
#4069 = LINE ( 'NONE', #2798, #4694 ) ;
#4070 = DIRECTION ( 'NONE',  ( -2.449021377849607626E-15, -3.265361837132810036E-15, -1.000000000000000000 ) ) ;
#4071 = CIRCLE ( 'NONE', #5950, 4.250000000000000000 ) ;
#4072 = CARTESIAN_POINT ( 'NONE',  ( 6.245824673232968749, 4.939548505212512097, -1.655093584846542010 ) ) ;
#4073 = PRODUCT_DEFINITION_SHAPE ( 'NONE', 'NONE',  #14635 ) ;
#4074 = CARTESIAN_POINT ( 'NONE',  ( 630.0000000000000000, 160.0000000000000284, -222.5000000000000000 ) ) ;
#4075 = AXIS2_PLACEMENT_3D ( 'NONE', #4217, #11944, #4080 ) ;
#4076 = DIRECTION ( 'NONE',  ( 0.000000000000000000, -1.000000000000000000, 0.000000000000000000 ) ) ;
#4077 = VERTEX_POINT ( 'NONE', #11202 ) ;
#4078 = CARTESIAN_POINT ( 'NONE',  ( 0.4465819873852049926, -5.773502691896264416, 5.911082023588295771E-17 ) ) ;
#4079 = CYLINDRICAL_SURFACE ( 'NONE', #14588, 4.250000000000000000 ) ;
#4080 = DIRECTION ( 'NONE',  ( -1.000000000000000000, 0.000000000000000000, 0.000000000000000000 ) ) ;
#4081 = PRESENTATION_LAYER_ASSIGNMENT (  '', '', ( #9504 ) ) ;
#4083 = CIRCLE ( 'NONE', #13988, 0.5155456020628804703 ) ;
#4082 = DIRECTION ( 'NONE',  ( 0.9578262852211513190, -0.2873478855663453846, 0.000000000000000000 ) ) ;
#4084 = ADVANCED_FACE ( 'NONE', ( #860 ), #14604, .T. ) ;
#4085 = VERTEX_POINT ( 'NONE', #14387 ) ;
#4086 = ORIENTED_EDGE ( 'NONE', *, *, #1036, .F. ) ;
#4087 = CARTESIAN_POINT ( 'NONE',  ( -6.259644161404860030E-16, -4.618802153517027165, -3.433295621305388234 ) ) ;
#4088 = LINE ( 'NONE', #3187, #12251 ) ;
#4089 = EDGE_CURVE ( 'NONE', #10470, #5125, #3903, .T. ) ;
#4090 = CARTESIAN_POINT ( 'NONE',  ( 6.357976367241986893, 5.421935536069748096, 0.8264656814052228073 ) ) ;
#4091 = B_SPLINE_CURVE_WITH_KNOTS ( 'NONE', 3,
 ( #11565, #1466, #5967, #3616 ),
 .UNSPECIFIED., .F., .F.,
 ( 4, 4 ),
 ( 2.380735200834041289E-07, 0.002921158011986723334 ),
 .UNSPECIFIED. ) ;
#4092 = AXIS2_PLACEMENT_3D ( 'NONE', #9935, #7491, #910 ) ;
#4093 = DIRECTION ( 'NONE',  ( 1.000000000000000000, 0.000000000000000000, 0.000000000000000000 ) ) ;
#4094 = ORIENTED_EDGE ( 'NONE', *, *, #10616, .F. ) ;
#4095 = VECTOR ( 'NONE', #12798, 1000.000000000000114 ) ;
#4096 = DIRECTION ( 'NONE',  ( 0.000000000000000000, 0.000000000000000000, 1.000000000000000000 ) ) ;
#4097 = CARTESIAN_POINT ( 'NONE',  ( 0.000000000000000000, 0.000000000000000000, -4.000000000000000000 ) ) ;
#4098 = CARTESIAN_POINT ( 'NONE',  ( 0.000000000000000000, 0.000000000000000000, 0.000000000000000000 ) ) ;
#4099 = ORIENTED_EDGE ( 'NONE', *, *, #3755, .T. ) ;
#4100 = EDGE_CURVE ( 'NONE', #902, #3137, #261, .T. ) ;
#4101 = DIRECTION ( 'NONE',  ( -0.9578262852211522071, 0.2873478855663427756, -9.629649721936179265E-30 ) ) ;
#4102 = CARTESIAN_POINT ( 'NONE',  ( 2.691179338796023329E-15, 4.647089433458991614, -3.572167766733753691 ) ) ;
#4103 = DIRECTION ( 'NONE',  ( -0.2873478855663452736, -0.9578262852211514300, 0.000000000000000000 ) ) ;
#4104 = EDGE_LOOP ( 'NONE', ( #2064, #12090, #5796, #4473 ) ) ;
#4105 = CARTESIAN_POINT ( 'NONE',  ( 639.4338945024659324, 161.8386352387035743, 211.0000000000000000 ) ) ;
#4106 = ORIENTED_EDGE ( 'NONE', *, *, #1193, .T. ) ;
#4107 = ORIENTED_EDGE ( 'NONE', *, *, #9548, .T. ) ;
#4108 = CARTESIAN_POINT ( 'NONE',  ( 1.250000000000000000, -6.429618962271402616, -1.000000000000000000 ) ) ;
#4109 = DIRECTION ( 'NONE',  ( -0.000000000000000000, 0.000000000000000000, 1.000000000000000000 ) ) ;
#4110 = ORIENTED_EDGE ( 'NONE', *, *, #6080, .T. ) ;
#4111 = ORIENTED_EDGE ( 'NONE', *, *, #5612, .F. ) ;
#4112 = FACE_OUTER_BOUND ( 'NONE', #9187, .T. ) ;
#4113 = EDGE_CURVE ( 'NONE', #72, #2660, #6985, .T. ) ;
#4114 = CARTESIAN_POINT ( 'NONE',  ( 627.5000000000000000, 160.9817477042468283, 210.0000120000000265 ) ) ;
#4115 = CARTESIAN_POINT ( 'NONE',  ( -1.996809568599176514E-13, 4.067926144610258734E-14, 182.7999999999994714 ) ) ;
#4116 = DIRECTION ( 'NONE',  ( -0.9578262852211507639, 0.2873478855663477716, -0.000000000000000000 ) ) ;
#4117 = VERTEX_POINT ( 'NONE', #4801 ) ;
#4118 = FACE_OUTER_BOUND ( 'NONE', #11843, .T. ) ;
#4119 = DIRECTION ( 'NONE',  ( 9.794481010665704304E-16, 3.264827003555234768E-15, -1.000000000000000000 ) ) ;
#4120 = ORIENTED_EDGE ( 'NONE', *, *, #3848, .F. ) ;
#4121 = ORIENTED_EDGE ( 'NONE', *, *, #12555, .T. ) ;
#4122 = DIRECTION ( 'NONE',  ( -1.148424442117026787E-15, 3.445273326351093279E-16, 1.000000000000000000 ) ) ;
#4123 = CARTESIAN_POINT ( 'NONE',  ( 635.0000000000000000, 160.0000000000000284, -222.5000000000000000 ) ) ;
#4124 = ORIENTED_EDGE ( 'NONE', *, *, #829, .F. ) ;
#4125 = CARTESIAN_POINT ( 'NONE',  ( 2.171643655288379993, -3.365003104552334978, -1.195831703456429434E-14 ) ) ;
#4126 = EDGE_CURVE ( 'NONE', #6460, #5688, #5193, .T. ) ;
#4127 = CARTESIAN_POINT ( 'NONE',  ( 635.0000000000000000, 160.0000000000000284, -217.5000000000000284 ) ) ;
#4128 = LINE ( 'NONE', #850, #10201 ) ;
#4129 = ORIENTED_EDGE ( 'NONE', *, *, #4466, .F. ) ;
#4130 = EDGE_CURVE ( 'NONE', #2290, #10969, #1253, .T. ) ;
#4131 = DIRECTION ( 'NONE',  ( 0.000000000000000000, 0.000000000000000000, 1.000000000000000000 ) ) ;
#4132 = CARTESIAN_POINT ( 'NONE',  ( -1.500000000000001332, 0.000000000000000000, 0.000000000000000000 ) ) ;
#4133 = ORIENTED_EDGE ( 'NONE', *, *, #7825, .T. ) ;
#4134 = EDGE_CURVE ( 'NONE', #6460, #442, #10528, .T. ) ;
#4135 = EDGE_CURVE ( 'NONE', #6803, #12905, #2647, .T. ) ;
#4136 = ORIENTED_EDGE ( 'NONE', *, *, #4337, .T. ) ;
#4137 = EDGE_CURVE ( 'NONE', #4046, #6408, #3537, .T. ) ;
#4138 = CARTESIAN_POINT ( 'NONE',  ( 635.0000000000000000, 160.0000000000000284, -210.0000000000000000 ) ) ;
#4139 = DIRECTION ( 'NONE',  ( 0.2873478855663454401, 0.9578262852211514300, 3.831370512995697396E-15 ) ) ;
#4140 = PLANE ( 'NONE',  #3558 ) ;
#4141 = UNCERTAINTY_MEASURE_WITH_UNIT (LENGTH_MEASURE( 1.000000000000000082E-05 ), #7997, 'distance_accuracy_value', 'NONE');
#4142 = DIRECTION ( 'NONE',  ( -0.000000000000000000, 0.000000000000000000, -1.000000000000000000 ) ) ;
#4143 = EDGE_LOOP ( 'NONE', ( #13847, #13186, #8940, #2515 ) ) ;
#4144 = CARTESIAN_POINT ( 'NONE',  ( 5.991014884144048480, -5.637851296924623057E-15, -5.000000000000000000 ) ) ;
#4145 = DIRECTION ( 'NONE',  ( 0.000000000000000000, -1.000000000000000000, 1.287488025362403787E-15 ) ) ;
#4146 = DIRECTION ( 'NONE',  ( -1.000000000000000000, 0.000000000000000000, 0.000000000000000000 ) ) ;
#4147 = EDGE_CURVE ( 'NONE', #7982, #7459, #4091, .T. ) ;
#4148 = EDGE_CURVE ( 'NONE', #7897, #13350, #8098, .T. ) ;
#4149 = CARTESIAN_POINT ( 'NONE',  ( 635.0000000000000000, 160.0000000000000284, -210.0000000000000000 ) ) ;
#4150 = ORIENTED_EDGE ( 'NONE', *, *, #5627, .T. ) ;
#4151 = ORIENTED_EDGE ( 'NONE', *, *, #4848, .F. ) ;
#4152 = DIRECTION ( 'NONE',  ( -0.5000000000000019984, -0.8660254037844375974, 0.000000000000000000 ) ) ;
#4153 = CARTESIAN_POINT ( 'NONE',  ( 139.8040310085880833, 355.9707293956415697, 210.0000000000000000 ) ) ;
#4154 = DIRECTION ( 'NONE',  ( 0.000000000000000000, 0.000000000000000000, 1.000000000000000000 ) ) ;
#4155 = DIRECTION ( 'NONE',  ( -0.9578262852211513190, 0.2873478855663453846, 0.000000000000000000 ) ) ;
#4156 = VERTEX_POINT ( 'NONE', #4642 ) ;
#4157 = ADVANCED_FACE ( 'NONE', ( #10467 ), #9357, .F. ) ;
#4158 = CARTESIAN_POINT ( 'NONE',  ( 5.384454397937118664, 0.000000000000000000, -4.484454397937119197 ) ) ;
#4159 = ORIENTED_EDGE ( 'NONE', *, *, #7179, .F. ) ;
#4160 = DIRECTION ( 'NONE',  ( 0.000000000000000000, 0.000000000000000000, 1.000000000000000000 ) ) ;
#4161 = CARTESIAN_POINT ( 'NONE',  ( -3.974357786152442180E-13, 4.796734841935204052, -3.721909803043259579 ) ) ;
#4162 = CARTESIAN_POINT ( 'NONE',  ( -0.5000000000000000000, -6.429618962271402616, -1.000000000000000000 ) ) ;
#4163 =( LENGTH_UNIT ( ) NAMED_UNIT ( * ) SI_UNIT ( .MILLI., .METRE. ) );
#4164 = ORIENTED_EDGE ( 'NONE', *, *, #8352, .F. ) ;
#4165 = FACE_OUTER_BOUND ( 'NONE', #10413, .T. ) ;
#4166 = VERTEX_POINT ( 'NONE', #13564 ) ;
#4167 = ORIENTED_EDGE ( 'NONE', *, *, #13136, .T. ) ;
#4168 = DIRECTION ( 'NONE',  ( -0.000000000000000000, -0.000000000000000000, 1.000000000000000000 ) ) ;
#4169 = CARTESIAN_POINT ( 'NONE',  ( 641.0000000000000000, 166.0000000000000284, 187.5000000000000000 ) ) ;
#4170 = EDGE_LOOP ( 'NONE', ( #9110, #12012 ) ) ;
#4171 = ORIENTED_EDGE ( 'NONE', *, *, #12076, .T. ) ;
#4172 = DIRECTION ( 'NONE',  ( 1.000000000000000000, 0.000000000000000000, 0.000000000000000000 ) ) ;
#4173 = LINE ( 'NONE', #6394, #12732 ) ;
#4174 = CARTESIAN_POINT ( 'NONE',  ( -1.748605424166683430E-13, -1.289150925701384681E-12, -182.7999999999981355 ) ) ;
#4175 = CARTESIAN_POINT ( 'NONE',  ( 630.0000000000000000, 160.0000000000000284, 211.0000000000000000 ) ) ;
#4176 = AXIS2_PLACEMENT_3D ( 'NONE', #7828, #13569, #9222 ) ;
#4177 = EDGE_LOOP ( 'NONE', ( #3386, #7778, #5979 ) ) ;
#4178 = DIRECTION ( 'NONE',  ( -0.000000000000000000, -0.000000000000000000, -1.000000000000000000 ) ) ;
#4179 = CONTEXT_DEPENDENT_SHAPE_REPRESENTATION ( #2168, #14450 ) ;
#4180 = ORIENTED_EDGE ( 'NONE', *, *, #11512, .F. ) ;
#4181 = PLANE ( 'NONE',  #988 ) ;
#4182 = VECTOR ( 'NONE', #8409, 1000.000000000000000 ) ;
#4183 = ORIENTED_EDGE ( 'NONE', *, *, #11310, .T. ) ;
#4184 = VECTOR ( 'NONE', #9342, 999.9999999999998863 ) ;
#4185 = EDGE_CURVE ( 'NONE', #8873, #11836, #5650, .T. ) ;
#4186 = CARTESIAN_POINT ( 'NONE',  ( -3.250000000000004441, 5.629165124598849879, 0.000000000000000000 ) ) ;
#4187 = FACE_OUTER_BOUND ( 'NONE', #464, .T. ) ;
#4188 = EDGE_LOOP ( 'NONE', ( #10021, #13008, #3979, #8499 ) ) ;
#4189 = CARTESIAN_POINT ( 'NONE',  ( 710.3801946911771665, 172.2695124801717270, 150.0000000000013358 ) ) ;
#4190 = DIRECTION ( 'NONE',  ( 0.000000000000000000, 0.000000000000000000, -1.000000000000000000 ) ) ;
#4191 = AXIS2_PLACEMENT_3D ( 'NONE', #12543, #2435, #9075 ) ;
#4192 = VECTOR ( 'NONE', #7930, 1000.000000000000000 ) ;
#4193 = CARTESIAN_POINT ( 'NONE',  ( 20.55500000000001748, 3.061616997868384127E-16, -2.500000000000000888 ) ) ;
#4194 = EDGE_LOOP ( 'NONE', ( #13696, #8382, #2322, #7933 ) ) ;
#4195 = CARTESIAN_POINT ( 'NONE',  ( 107.2182642636026202, 357.3942142120087055, -210.0000000000000000 ) ) ;
#4196 = CARTESIAN_POINT ( 'NONE',  ( -6.500000000000000888, 0.000000000000000000, 0.000000000000000000 ) ) ;
#4197 = VERTEX_POINT ( 'NONE', #12603 ) ;
#4198 = ORIENTED_EDGE ( 'NONE', *, *, #157, .F. ) ;
#4199 = CARTESIAN_POINT ( 'NONE',  ( 4.211140560182196957, -2.431303136016555122, -3.745885042887436622 ) ) ;
#4200 = EDGE_CURVE ( 'NONE', #13817, #443, #13856, .T. ) ;
#4201 = VECTOR ( 'NONE', #5111, 1000.000000000000000 ) ;
#4203 = AXIS2_PLACEMENT_3D ( 'NONE', #8824, #8470, #8883 ) ;
#4202 = CARTESIAN_POINT ( 'NONE',  ( -10.00000000000045297, 371.6790804732678453, -1.178702027242996938E-12 ) ) ;
#4204 = EDGE_CURVE ( 'NONE', #2553, #2452, #4727, .T. ) ;
#4205 = CARTESIAN_POINT ( 'NONE',  ( 6.095473853218515536, 4.853892138986622307, -1.592812200815997059 ) ) ;
#4206 = CARTESIAN_POINT ( 'NONE',  ( -3.999999999999999112, -2.309401076758512694, -3.504269196027871125 ) ) ;
#4207 = EDGE_CURVE ( 'NONE', #3684, #7897, #12754, .T. ) ;
#4208 = ADVANCED_BREP_SHAPE_REPRESENTATION ( '', ( #7105, #9440 ), #5461 ) ;
#4209 = CARTESIAN_POINT ( 'NONE',  ( 703.1581845006096501, 166.2926764603917036, -177.6000000000005059 ) ) ;
#4210 = ORIENTED_EDGE ( 'NONE', *, *, #6506, .F. ) ;
#4211 = VECTOR ( 'NONE', #7603, 1000.000000000000000 ) ;
#4212 = EDGE_CURVE ( 'NONE', #11364, #6968, #12008, .T. ) ;
#4213 = VECTOR ( 'NONE', #1863, 999.9999999999998863 ) ;
#4214 = AXIS2_PLACEMENT_3D ( 'NONE', #9315, #12336, #3482 ) ;
#4215 = CARTESIAN_POINT ( 'NONE',  ( 6.367873360227556567, 2.886751345948122882, -5.000000000000000000 ) ) ;
#4216 = CARTESIAN_POINT ( 'NONE',  ( 6.534838248920900483, -5.903531555104837736, 5.201568163584232486E-16 ) ) ;
#4217 = CARTESIAN_POINT ( 'NONE',  ( 446.3084422793565409, 264.0194060144110608, -215.0000000000000000 ) ) ;
#4218 = CARTESIAN_POINT ( 'NONE',  ( 103.3965373855728558, 344.6551246185656510, -190.0000000000000000 ) ) ;
#4219 = ORIENTED_EDGE ( 'NONE', *, *, #6873, .F. ) ;
#4220 = EDGE_LOOP ( 'NONE', ( #1177, #14051, #6741, #4063, #7686, #11712, #2508 ) ) ;
#4221 = CARTESIAN_POINT ( 'NONE',  ( 33.05499999999999972, 3.061616997868383634E-16, -2.500000000000000444 ) ) ;
#4222 = LINE ( 'NONE', #14330, #6847 ) ;
#4223 = CARTESIAN_POINT ( 'NONE',  ( 6.390983399715593372, 5.837459000499768180, -0.1107755759658281131 ) ) ;
#4224 = AXIS2_PLACEMENT_3D ( 'NONE', #7025, #3871, #2682 ) ;
#4225 = CIRCLE ( 'NONE', #4706, 5.199999999999707079 ) ;
#4226 = CARTESIAN_POINT ( 'NONE',  ( 650.0000000000000000, 175.0000000000000568, 210.0000000000000000 ) ) ;
#4227 = ORIENTED_EDGE ( 'NONE', *, *, #14325, .T. ) ;
#4228 = EDGE_CURVE ( 'NONE', #443, #4433, #4051, .T. ) ;
#4229 = CARTESIAN_POINT ( 'NONE',  ( -6.500000000000000000, -1.336926445777093964, -6.054363369342815382 ) ) ;
#4230 = ORIENTED_EDGE ( 'NONE', *, *, #14561, .T. ) ;
#4231 =( GEOMETRIC_REPRESENTATION_CONTEXT ( 3 ) GLOBAL_UNCERTAINTY_ASSIGNED_CONTEXT ( ( #595 ) ) GLOBAL_UNIT_ASSIGNED_CONTEXT ( ( #7441, #4947, #718 ) ) REPRESENTATION_CONTEXT ( 'NONE', 'WORKASPACE' ) );
#4232 = EDGE_CURVE ( 'NONE', #681, #12648, #2865, .T. ) ;
#4233 = LINE ( 'NONE', #13453, #3494 ) ;
#4234 = CARTESIAN_POINT ( 'NONE',  ( -2.262848203703084593, -6.566616684922157887, -6.208169345099794789 ) ) ;
#4235 = CARTESIAN_POINT ( 'NONE',  ( 2.500000000000000000, 2.357898499370431722, -2.818925648462311528E-15 ) ) ;
#4236 = VERTEX_POINT ( 'NONE', #4935 ) ;
#4237 = VECTOR ( 'NONE', #13070, 1000.000000000000000 ) ;
#4238 = CARTESIAN_POINT ( 'NONE',  ( 3.098410542199072637, -7.060458129626440815, -1.000000000000000000 ) ) ;
#4239 = AXIS2_PLACEMENT_3D ( 'NONE', #13555, #93, #5798 ) ;
#4240 = ORIENTED_EDGE ( 'NONE', *, *, #8287, .T. ) ;
#4241 = EDGE_LOOP ( 'NONE', ( #6674, #9406, #1655, #7629, #7207 ) ) ;
#4242 = CARTESIAN_POINT ( 'NONE',  ( 470.8287951810180516, 310.9528939902474463, 210.0000000000000000 ) ) ;
#4243 = B_SPLINE_CURVE_WITH_KNOTS ( 'NONE', 3,
 ( #6370, #8168, #13568, #184, #6929, #11209 ),
 .UNSPECIFIED., .F., .F.,
 ( 4, 2, 4 ),
 ( 0.003981881017442828914, 0.005970145066490142871, 0.007958409115537457695 ),
 .UNSPECIFIED. ) ;
#4244 = DIRECTION ( 'NONE',  ( -0.2873478855662748299, -0.9578262852211725242, -1.261617073437831000E-13 ) ) ;
#4245 = AXIS2_PLACEMENT_3D ( 'NONE', #6695, #7586, #784 ) ;
#4246 = VERTEX_POINT ( 'NONE', #10909 ) ;
#4247 = AXIS2_PLACEMENT_3D ( 'NONE', #2703, #1366, #6019 ) ;
#4248 = ORIENTED_EDGE ( 'NONE', *, *, #13992, .T. ) ;
#4249 = FACE_BOUND ( 'NONE', #7347, .T. ) ;
#4250 = DIRECTION ( 'NONE',  ( -0.000000000000000000, -0.000000000000000000, 1.000000000000000000 ) ) ;
#4251 = CARTESIAN_POINT ( 'NONE',  ( 459.7035746174795463, 294.6698471414878782, -190.0000000000000568 ) ) ;
#4252 = DIRECTION ( 'NONE',  ( -0.2873478855663453291, -0.9578262852211513190, 3.835990623682899812E-15 ) ) ;
#4253 = DIRECTION ( 'NONE',  ( -0.9237280213470682178, -0.3830490080632377725, 0.000000000000000000 ) ) ;
#4254 = FILL_AREA_STYLE_COLOUR ( '', #8762 ) ;
#4255 = CIRCLE ( 'NONE', #10855, 4.799999999999968736 ) ;
#4256 = ORIENTED_EDGE ( 'NONE', *, *, #2498, .F. ) ;
#4257 = AXIS2_PLACEMENT_3D ( 'NONE', #4674, #5553, #6801 ) ;
#4258 = CARTESIAN_POINT ( 'NONE',  ( -1.250000000000000000, -6.429618962271402616, -1.000000000000000000 ) ) ;
#4259 = VERTEX_POINT ( 'NONE', #563 ) ;
#4260 = LINE ( 'NONE', #13265, #4038 ) ;
#4261 = AXIS2_PLACEMENT_3D ( 'NONE', #9619, #4015, #13020 ) ;
#4262 = ORIENTED_EDGE ( 'NONE', *, *, #6737, .F. ) ;
#4263 = EDGE_CURVE ( 'NONE', #12176, #5143, #11440, .T. ) ;
#4264 = CARTESIAN_POINT ( 'NONE',  ( -1.400000000000001910, 6.123233995736766282E-16, 5.000000000000000000 ) ) ;
#4265 = CIRCLE ( 'NONE', #1437, 2.649999999999985700 ) ;
#4266 = CIRCLE ( 'NONE', #9679, 4.200000000000009059 ) ;
#4267 = LINE ( 'NONE', #8770, #9464 ) ;
#4268 = ORIENTED_EDGE ( 'NONE', *, *, #11858, .F. ) ;
#4269 = CARTESIAN_POINT ( 'NONE',  ( 610.7462142612635034, 188.6189422762846561, 185.0840554379255707 ) ) ;
#4270 = LINE ( 'NONE', #925, #7994 ) ;
#4271 = AXIS2_PLACEMENT_3D ( 'NONE', #140, #13965, #5037 ) ;
#4272 = DIRECTION ( 'NONE',  ( 0.2873478855663418874, 0.9578262852211524292, 0.000000000000000000 ) ) ;
#4273 = PRESENTATION_STYLE_ASSIGNMENT (( #14522 ) ) ;
#4274 = EDGE_LOOP ( 'NONE', ( #7569, #11902, #13356, #7417 ) ) ;
#4276 = EDGE_CURVE ( 'NONE', #11781, #11591, #13439, .T. ) ;
#4275 = DIRECTION ( 'NONE',  ( -0.9578262852211498757, 0.2873478855663503251, -1.198990317802636355E-15 ) ) ;
#4277 = ORIENTED_EDGE ( 'NONE', *, *, #4714, .F. ) ;
#4278 = CIRCLE ( 'NONE', #4762, 8.105212085995399107 ) ;
#4279 = VECTOR ( 'NONE', #1612, 1000.000000000000000 ) ;
#4280 = VERTEX_POINT ( 'NONE', #10829 ) ;
#4281 = LINE ( 'NONE', #13499, #9631 ) ;
#4282 = AXIS2_PLACEMENT_3D ( 'NONE', #9414, #383, #10373 ) ;
#4283 = PRESENTATION_LAYER_ASSIGNMENT (  '', '', ( #11810 ) ) ;
#4284 = CARTESIAN_POINT ( 'NONE',  ( 627.5000000000000000, 160.0000000000000284, -210.0000059999999849 ) ) ;
#4285 = CARTESIAN_POINT ( 'NONE',  ( -6.473970235329672780E-16, -4.862606272033106691, -3.745885042887442395 ) ) ;
#4286 = CONICAL_SURFACE ( 'NONE', #13467, 3.999999999999999112, 0.9599310885968813656 ) ;
#4287 = CARTESIAN_POINT ( 'NONE',  ( -1.400000000000001910, 0.000000000000000000, -5.000000000000000000 ) ) ;
#4288 = PRODUCT_DEFINITION_CONTEXT ( 'detailed design', #9333, 'design' ) ;
#4289 = LINE ( 'NONE', #1921, #9835 ) ;
#4290 = ADVANCED_FACE ( 'NONE', ( #11700 ), #686, .T. ) ;
#4291 = ORIENTED_EDGE ( 'NONE', *, *, #14225, .T. ) ;
#4292 = FACE_OUTER_BOUND ( 'NONE', #1358, .T. ) ;
#4293 = DIRECTION ( 'NONE',  ( 0.1305261922200524616, -0.9914448613738103822, 0.000000000000000000 ) ) ;
#4294 = APPLICATION_PROTOCOL_DEFINITION ( 'draft international standard', 'automotive_design', 1998, #7830 ) ;
#4295 = CARTESIAN_POINT ( 'NONE',  ( 635.0000000000000000, 160.0000000000000284, 211.0000000000000000 ) ) ;
#4296 = VERTEX_POINT ( 'NONE', #8317 ) ;
#4297 = EDGE_LOOP ( 'NONE', ( #4001, #7640, #2738, #7734, #9118, #3370, #4712 ) ) ;
#4298 = VECTOR ( 'NONE', #6911, 1000.000000000000000 ) ;
#4299 =( LENGTH_UNIT ( ) NAMED_UNIT ( * ) SI_UNIT ( .MILLI., .METRE. ) );
#4300 = DIRECTION ( 'NONE',  ( 0.000000000000000000, 0.000000000000000000, -1.000000000000000000 ) ) ;
#4301 = LINE ( 'NONE', #12466, #13187 ) ;
#4302 = AXIS2_PLACEMENT_3D ( 'NONE', #1925, #11883, #6436 ) ;
#4303 = CARTESIAN_POINT ( 'NONE',  ( 610.8620436566991430, 188.5525593289318351, -169.9999999999999716 ) ) ;
#4304 = VERTEX_POINT ( 'NONE', #10688 ) ;
#4305 = ADVANCED_FACE ( 'NONE', ( #6252 ), #9428, .T. ) ;
#4306 = AXIS2_PLACEMENT_3D ( 'NONE', #12833, #10755, #633 ) ;
#4307 = CARTESIAN_POINT ( 'NONE',  ( -6.838238953609876880, 3.993985489099932007, -6.572971244646267586 ) ) ;
#4308 = EDGE_CURVE ( 'NONE', #9854, #4571, #1893, .T. ) ;
#4309 = EDGE_LOOP ( 'NONE', ( #2457, #9771, #1731 ) ) ;
#4310 = AXIS2_PLACEMENT_3D ( 'NONE', #1564, #4983, #13823 ) ;
#4311 = DIRECTION ( 'NONE',  ( -0.9578262852211499867, 0.2873478855663502696, -1.489419751501264127E-15 ) ) ;
#4312 = CARTESIAN_POINT ( 'NONE',  ( 635.0000000000000000, 160.0000000000000284, 211.0000000000000000 ) ) ;
#4313 = CARTESIAN_POINT ( 'NONE',  ( -20.63749999999999574, 9.184850993605147944E-16, 7.500000000000000000 ) ) ;
#4314 = PRESENTATION_STYLE_ASSIGNMENT (( #5198 ) ) ;
#4315 = ORIENTED_EDGE ( 'NONE', *, *, #7922, .F. ) ;
#4316 = DIRECTION ( 'NONE',  ( 0.000000000000000000, 0.000000000000000000, 1.000000000000000000 ) ) ;
#4317 = EDGE_LOOP ( 'NONE', ( #845, #4133 ) ) ;
#4318 = ORIENTED_EDGE ( 'NONE', *, *, #12783, .T. ) ;
#4319 = EDGE_CURVE ( 'NONE', #7886, #13629, #9192, .T. ) ;
#4320 = CARTESIAN_POINT ( 'NONE',  ( -4.211140560182196957, 2.431303136016537803, -3.745885042887433514 ) ) ;
#4321 = EDGE_CURVE ( 'NONE', #2113, #151, #6602, .T. ) ;
#4322 = FACE_OUTER_BOUND ( 'NONE', #12634, .T. ) ;
#4323 = VECTOR ( 'NONE', #7274, 1000.000000000000000 ) ;
#4324 = EDGE_CURVE ( 'NONE', #352, #14524, #9514, .T. ) ;
#4325 = VERTEX_POINT ( 'NONE', #6188 ) ;
#4326 = EDGE_LOOP ( 'NONE', ( #3946, #4240, #10995, #8931 ) ) ;
#4327 = CARTESIAN_POINT ( 'NONE',  ( 6.500000000000000000, -3.752776749732574135, -6.064240316920400886 ) ) ;
#4328 = DIRECTION ( 'NONE',  ( 0.000000000000000000, 0.000000000000000000, 1.000000000000000000 ) ) ;
#4329 = DIRECTION ( 'NONE',  ( 0.000000000000000000, 0.000000000000000000, -1.000000000000000000 ) ) ;
#4330 = DIRECTION ( 'NONE',  ( 0.000000000000000000, -1.000000000000000000, 0.000000000000000000 ) ) ;
#4331 = SHAPE_REPRESENTATION_RELATIONSHIP ( 'NONE' , 'NONE' ,  #342, #8625 ) ;
#4332 = ORIENTED_EDGE ( 'NONE', *, *, #13781, .F. ) ;
#4333 = CARTESIAN_POINT ( 'NONE',  ( 610.0000000000001137, 191.1080398579018720, 190.0000000000000000 ) ) ;
#4334 = ORIENTED_EDGE ( 'NONE', *, *, #3310, .F. ) ;
#4335 = CARTESIAN_POINT ( 'NONE',  ( -10.00000000000000000, -10.00000000000000000, 210.0000000000000000 ) ) ;
#4336 = B_SPLINE_CURVE_WITH_KNOTS ( 'NONE', 3,
 ( #4975, #9475, #13979, #13674, #3869 ),
 .UNSPECIFIED., .F., .F.,
 ( 4, 1, 4 ),
 ( 0.000000000000000000, 0.002309401076758505790, 0.004618802153517011580 ),
 .UNSPECIFIED. ) ;
#4337 = EDGE_CURVE ( 'NONE', #6378, #2860, #12329, .T. ) ;
#4338 = ORIENTED_EDGE ( 'NONE', *, *, #4667, .F. ) ;
#4339 = FACE_OUTER_BOUND ( 'NONE', #7857, .T. ) ;
#4340 = APPLICATION_CONTEXT ( 'automotive_design' ) ;
#4341 = CARTESIAN_POINT ( 'NONE',  ( -10.00000000000000000, 413.4403065089105667, -210.0000000000000000 ) ) ;
#4342 = ORIENTED_EDGE ( 'NONE', *, *, #8898, .T. ) ;
#4343 = CARTESIAN_POINT ( 'NONE',  ( 446.3084422793565409, 264.0194060144110608, -190.0000000000000000 ) ) ;
#4344 = LINE ( 'NONE', #3165, #920 ) ;
#4345 = EDGE_CURVE ( 'NONE', #808, #1059, #7584, .T. ) ;
#4346 = LINE ( 'NONE', #7593, #2416 ) ;
#4347 = CARTESIAN_POINT ( 'NONE',  ( 0.000000000000000000, 0.000000000000000000, 0.000000000000000000 ) ) ;
#4348 = ORIENTED_EDGE ( 'NONE', *, *, #11146, .T. ) ;
#4349 = ADVANCED_FACE ( 'NONE', ( #8461 ), #707, .F. ) ;
#4350 = FACE_OUTER_BOUND ( 'NONE', #666, .T. ) ;
#4351 = ORIENTED_EDGE ( 'NONE', *, *, #7821, .T. ) ;
#4352 = VERTEX_POINT ( 'NONE', #9731 ) ;
#4353 = CARTESIAN_POINT ( 'NONE',  ( 640.0000000000000000, 160.0000000000000284, 215.5000000000000000 ) ) ;
#4354 = CARTESIAN_POINT ( 'NONE',  ( -20.63749999999999574, 0.000000000000000000, 0.000000000000000000 ) ) ;
#4355 = DIRECTION ( 'NONE',  ( -2.449021377849607626E-15, -3.265361837132810036E-15, -1.000000000000000000 ) ) ;
#4356 = EDGE_CURVE ( 'NONE', #8976, #1995, #455, .T. ) ;
#4357 = AXIS2_PLACEMENT_3D ( 'NONE', #2348, #5533, #1318 ) ;
#4358 = DIRECTION ( 'NONE',  ( 1.000000000000000000, -3.469446951953611033E-15, -0.000000000000000000 ) ) ;
#4359 = CARTESIAN_POINT ( 'NONE',  ( 6.878751942472531411, 3.924677726130922473, -6.573129608219089981 ) ) ;
#4360 = DIRECTION ( 'NONE',  ( -0.000000000000000000, -0.000000000000000000, -1.000000000000000000 ) ) ;
#4361 = CARTESIAN_POINT ( 'NONE',  ( 639.0000000000000000, 156.0000000000000000, -233.5000000000000000 ) ) ;
#4362 = ORIENTED_EDGE ( 'NONE', *, *, #12248, .F. ) ;
#4363 = DIRECTION ( 'NONE',  ( -0.000000000000000000, -0.000000000000000000, 1.000000000000000000 ) ) ;
#4364 = CARTESIAN_POINT ( 'NONE',  ( 6.534838248920899595, -2.951765777552421532, -5.112608298763837489 ) ) ;
#4365 = APPLICATION_PROTOCOL_DEFINITION ( 'draft international standard', 'automotive_design', 1998, #12344 ) ;
#4366 = PLANE ( 'NONE',  #221 ) ;
#4367 = ORIENTED_EDGE ( 'NONE', *, *, #1726, .F. ) ;
#4368 = ORIENTED_EDGE ( 'NONE', *, *, #13041, .T. ) ;
#4369 = DIRECTION ( 'NONE',  ( 1.000000000000000000, 0.000000000000000000, 0.000000000000000000 ) ) ;
#4370 = DIRECTION ( 'NONE',  ( -0.000000000000000000, -0.000000000000000000, 1.000000000000000000 ) ) ;
#4371 = EDGE_CURVE ( 'NONE', #11023, #11723, #11075, .T. ) ;
#4372 = CARTESIAN_POINT ( 'NONE',  ( -5.619193549421041212, 4.261310591078285803, -5.875704392894027350 ) ) ;
#4373 = ORIENTED_EDGE ( 'NONE', *, *, #7319, .F. ) ;
#4374 = CARTESIAN_POINT ( 'NONE',  ( 642.0000000000000000, 235.0000000000000284, -233.5000000000000000 ) ) ;
#4375 = VERTEX_POINT ( 'NONE', #3080 ) ;
#4376 = DIRECTION ( 'NONE',  ( -0.9578262852211506528, 0.2873478855663477161, -0.000000000000000000 ) ) ;
#4377 = DIRECTION ( 'NONE',  ( -1.000000000000000000, 0.000000000000000000, 0.000000000000000000 ) ) ;
#4378 = DIRECTION ( 'NONE',  ( 1.000000000000000000, 0.000000000000000000, 0.000000000000000000 ) ) ;
#4379 = ORIENTED_EDGE ( 'NONE', *, *, #4583, .T. ) ;
#4380 = EDGE_LOOP ( 'NONE', ( #3757, #3450, #5668, #10845 ) ) ;
#4381 = CARTESIAN_POINT ( 'NONE',  ( -1.999999999999999556, 3.464101615137754830, -3.142992957459232795 ) ) ;
#4382 = FACE_OUTER_BOUND ( 'NONE', #14060, .T. ) ;
#4383 = EDGE_CURVE ( 'NONE', #8575, #9997, #6622, .T. ) ;
#4384 = DIRECTION ( 'NONE',  ( -1.000000000000000000, 0.000000000000000000, 0.000000000000000000 ) ) ;
#4385 = EDGE_CURVE ( 'NONE', #8837, #1371, #1069, .T. ) ;
#4386 = ORIENTED_EDGE ( 'NONE', *, *, #14350, .F. ) ;
#4387 = ORIENTED_EDGE ( 'NONE', *, *, #10706, .F. ) ;
#4388 = DIRECTION ( 'NONE',  ( 0.000000000000000000, 0.000000000000000000, 1.000000000000000000 ) ) ;
#4389 = DIRECTION ( 'NONE',  ( -1.000000000000000000, -9.498873539028489960E-17, 0.000000000000000000 ) ) ;
#4390 = EDGE_CURVE ( 'NONE', #11464, #1949, #11189, .T. ) ;
#4391 = CARTESIAN_POINT ( 'NONE',  ( 627.5000000000000000, 160.0000000000000284, -225.5000000000000000 ) ) ;
#4392 = CARTESIAN_POINT ( 'NONE',  ( 1.600000000000000089, 8.572527594031473190E-16, -7.000000000000000000 ) ) ;
#4393 = FACE_OUTER_BOUND ( 'NONE', #12263, .T. ) ;
#4394 = SURFACE_SIDE_STYLE ('',( #13610 ) ) ;
#4395 = PRODUCT_DEFINITION_SHAPE ( 'NONE', 'NONE',  #9740 ) ;
#4396 = ORIENTED_EDGE ( 'NONE', *, *, #7209, .T. ) ;
#4397 = EDGE_CURVE ( 'NONE', #8837, #7674, #8721, .T. ) ;
#4398 = DIRECTION ( 'NONE',  ( 0.000000000000000000, 0.000000000000000000, 1.000000000000000000 ) ) ;
#4399 = ORIENTED_EDGE ( 'NONE', *, *, #11764, .T. ) ;
#4400 = EDGE_LOOP ( 'NONE', ( #8592, #2525 ) ) ;
#4401 = DIRECTION ( 'NONE',  ( 1.000000000000000000, 0.000000000000000000, 0.000000000000000000 ) ) ;
#4402 = ORIENTED_EDGE ( 'NONE', *, *, #2759, .F. ) ;
#4403 = CARTESIAN_POINT ( 'NONE',  ( 0.000000000000000000, 0.000000000000000000, 0.000000000000000000 ) ) ;
#4404 = DIRECTION ( 'NONE',  ( -1.000000000000000000, 0.000000000000000000, 0.000000000000000000 ) ) ;
#4405 = ORIENTED_EDGE ( 'NONE', *, *, #6481, .F. ) ;
#4406 = CYLINDRICAL_SURFACE ( 'NONE', #9944, 6.080745460913608902 ) ;
#4407 = DIRECTION ( 'NONE',  ( 0.000000000000000000, 0.000000000000000000, 1.000000000000000000 ) ) ;
#4408 = ADVANCED_FACE ( 'NONE', ( #5516 ), #8484, .F. ) ;
#4409 = EDGE_CURVE ( 'NONE', #6536, #5458, #4474, .T. ) ;
#4410 = CARTESIAN_POINT ( 'NONE',  ( 630.0000000000000000, 160.0000000000000284, -211.0000000000000000 ) ) ;
#4411 = ORIENTED_EDGE ( 'NONE', *, *, #12861, .F. ) ;
#4412 = EDGE_CURVE ( 'NONE', #7148, #4236, #12079, .T. ) ;
#4413 = CARTESIAN_POINT ( 'NONE',  ( 6.445127866599366762, 5.657054305385774917, 0.4229901806197435277 ) ) ;
#4414 = ORIENTED_EDGE ( 'NONE', *, *, #7448, .F. ) ;
#4415 = EDGE_LOOP ( 'NONE', ( #3985, #2706, #4386, #9688 ) ) ;
#4416 = DIRECTION ( 'NONE',  ( -0.000000000000000000, -0.000000000000000000, -1.000000000000000000 ) ) ;
#4417 = FACE_BOUND ( 'NONE', #277, .T. ) ;
#4418 = CARTESIAN_POINT ( 'NONE',  ( 1.747541505913279281, -3.837784562140273081, -3.503702292528912299 ) ) ;
#4419 = AXIS2_PLACEMENT_3D ( 'NONE', #13926, #3823, #14067 ) ;
#4420 = AXIS2_PLACEMENT_3D ( 'NONE', #11536, #10441, #369 ) ;
#4421 = CARTESIAN_POINT ( 'NONE',  ( 148.9991633467111569, 386.6211705227183870, -210.0000000000000000 ) ) ;
#4422 = CIRCLE ( 'NONE', #11953, 2.700000000000000178 ) ;
#4423 = CARTESIAN_POINT ( 'NONE',  ( 2.075968632158072591, 6.306992450858666110, -6.056431503347234013 ) ) ;
#4424 = LINE ( 'NONE', #3241, #1429 ) ;
#4425 = CARTESIAN_POINT ( 'NONE',  ( 124.4591373975839304, 414.8637913252777025, 0.000000000000000000 ) ) ;
#4426 = ORIENTED_EDGE ( 'NONE', *, *, #9906, .F. ) ;
#4427 = CARTESIAN_POINT ( 'NONE',  ( -2.075968632161005800, -6.306992450858350807, -6.056431503346042078 ) ) ;
#4428 = DIRECTION ( 'NONE',  ( -1.000000000000000000, 0.000000000000000000, -1.148424442117026787E-15 ) ) ;
#4429 = SHAPE_DEFINITION_REPRESENTATION ( #12775, #1873 ) ;
#4430 =( GEOMETRIC_REPRESENTATION_CONTEXT ( 3 ) GLOBAL_UNCERTAINTY_ASSIGNED_CONTEXT ( ( #1937 ) ) GLOBAL_UNIT_ASSIGNED_CONTEXT ( ( #10196, #14542, #13437 ) ) REPRESENTATION_CONTEXT ( 'NONE', 'WORKASPACE' ) );
#4431 = DIRECTION ( 'NONE',  ( 1.000000000000000000, 0.000000000000000000, 0.000000000000000000 ) ) ;
#4432 = AXIS2_PLACEMENT_3D ( 'NONE', #12803, #8428, #9331 ) ;
#4433 = VERTEX_POINT ( 'NONE', #6754 ) ;
#4434 = ORIENTED_EDGE ( 'NONE', *, *, #1395, .F. ) ;
#4435 = CARTESIAN_POINT ( 'NONE',  ( 0.000000000000000000, 0.000000000000000000, -1.000000000000000000 ) ) ;
#4436 = LINE ( 'NONE', #2504, #10591 ) ;
#4437 =( REPRESENTATION_RELATIONSHIP ('NONE','NONE', #2822, #6779 ) REPRESENTATION_RELATIONSHIP_WITH_TRANSFORMATION ( #839 )SHAPE_REPRESENTATION_RELATIONSHIP( ) );
#4438 = CARTESIAN_POINT ( 'NONE',  ( 630.0000000000000000, 160.0000000000000284, 210.0000000000000000 ) ) ;
#4440 = ORIENTED_EDGE ( 'NONE', *, *, #8034, .F. ) ;
#4439 = PRESENTATION_LAYER_ASSIGNMENT (  '', '', ( #651 ) ) ;
#4441 = VECTOR ( 'NONE', #8806, 1000.000000000000000 ) ;
#4442 = CARTESIAN_POINT ( 'NONE',  ( 6.212068001622697011, -3.310128279683407282, -4.266689640017786722 ) ) ;
#4443 = EDGE_LOOP ( 'NONE', ( #11982, #9286, #115, #6846 ) ) ;
#4444 = CARTESIAN_POINT ( 'NONE',  ( 446.3084422793565409, 264.0194060144110608, 187.0000000000000000 ) ) ;
#4445 = CARTESIAN_POINT ( 'NONE',  ( 635.0000000000000000, 160.0000000000000284, -217.5000000000000284 ) ) ;
#4446 = EDGE_CURVE ( 'NONE', #14275, #9080, #1971, .T. ) ;
#4447 = DIRECTION ( 'NONE',  ( -0.000000000000000000, -0.000000000000000000, -1.000000000000000000 ) ) ;
#4448 = EDGE_CURVE ( 'NONE', #6337, #14518, #9795, .T. ) ;
#4449 = EDGE_LOOP ( 'NONE', ( #11541, #10923, #337, #8576 ) ) ;
#4450 = VERTEX_POINT ( 'NONE', #843 ) ;
#4451 = DIRECTION ( 'NONE',  ( 1.000000000000000000, 0.000000000000000000, 0.000000000000000000 ) ) ;
#4452 = AXIS2_PLACEMENT_3D ( 'NONE', #12407, #13597, #5496 ) ;
#4453 = AXIS2_PLACEMENT_3D ( 'NONE', #9724, #4119, #11992 ) ;
#4454 = DIRECTION ( 'NONE',  ( 0.000000000000000000, 0.000000000000000000, -1.000000000000000000 ) ) ;
#4455 = CARTESIAN_POINT ( 'NONE',  ( 610.0000000000000000, 227.4403065089105951, 190.0000000000000000 ) ) ;
#4456 = AXIS2_PLACEMENT_3D ( 'NONE', #271, #13647, #3543 ) ;
#4457 = ORIENTED_EDGE ( 'NONE', *, *, #10901, .F. ) ;
#4458 = ORIENTED_EDGE ( 'NONE', *, *, #1046, .F. ) ;
#4459 = CARTESIAN_POINT ( 'NONE',  ( 609.9289135522120660, 190.4185930515760958, -190.0000000000000284 ) ) ;
#4460 = DIRECTION ( 'NONE',  ( -0.9578262852211513190, 0.2873478855663453846, 0.000000000000000000 ) ) ;
#4461 = AXIS2_PLACEMENT_3D ( 'NONE', #13419, #10023, #3101 ) ;
#4462 = CARTESIAN_POINT ( 'NONE',  ( -3.455068668934486276, 2.624017327439035707, -3.316620875263955437 ) ) ;
#4463 = DIRECTION ( 'NONE',  ( 0.000000000000000000, -1.000000000000000000, 0.000000000000000000 ) ) ;
#4464 = SURFACE_SIDE_STYLE ('',( #7870 ) ) ;
#4465 =( NAMED_UNIT ( * ) SI_UNIT ( $, .STERADIAN. ) SOLID_ANGLE_UNIT ( ) );
#4466 = EDGE_CURVE ( 'NONE', #7506, #2990, #3160, .T. ) ;
#4467 = ORIENTED_EDGE ( 'NONE', *, *, #6837, .T. ) ;
#4468 = CARTESIAN_POINT ( 'NONE',  ( 446.3084422793565409, 264.0194060144110608, -190.0000000000000000 ) ) ;
#4469 = ORIENTED_EDGE ( 'NONE', *, *, #9319, .F. ) ;
#4470 = ORIENTED_EDGE ( 'NONE', *, *, #6275, .T. ) ;
#4471 = CARTESIAN_POINT ( 'NONE',  ( -2.500000000000000444, 3.061616997868383634E-16, -5.000000000000000888 ) ) ;
#4472 = VECTOR ( 'NONE', #1458, 1000.000000000000000 ) ;
#4473 = ORIENTED_EDGE ( 'NONE', *, *, #2986, .T. ) ;
#4474 = CIRCLE ( 'NONE', #2109, 7.500000000000000000 ) ;
#4475 = EDGE_CURVE ( 'NONE', #2146, #14514, #12247, .T. ) ;
#4476 = VECTOR ( 'NONE', #7665, 1000.000000000000000 ) ;
#4477 = FACE_OUTER_BOUND ( 'NONE', #6259, .T. ) ;
#4478 = B_SPLINE_CURVE_WITH_KNOTS ( 'NONE', 3,
 ( #6998, #2934, #10323, #12890, #10747, #1392, #2777, #5897, #10604, #11768, #487, #3900, #1677, #6183, #5081, #9576 ),
 .UNSPECIFIED., .F., .F.,
 ( 4, 3, 3, 3, 3, 4 ),
 ( -2.669610558406018255E-06, 0.000000000000000000, 5.703179328865577653E-05, 0.0001157653700801011267, 0.0001686517580788931929, 0.0002219032271218163556 ),
 .UNSPECIFIED. ) ;
#4479 = CARTESIAN_POINT ( 'NONE',  ( 703.1581845006096501, 166.2926764603917036, -177.6000000000005059 ) ) ;
#4480 = AXIS2_PLACEMENT_3D ( 'NONE', #13675, #12570, #4451 ) ;
#4481 = EDGE_LOOP ( 'NONE', ( #4754, #13739, #9861, #13102 ) ) ;
#4482 = FACE_OUTER_BOUND ( 'NONE', #13027, .T. ) ;
#4483 = DIRECTION ( 'NONE',  ( 1.000000000000000000, 0.000000000000000000, 0.000000000000000000 ) ) ;
#4484 = CIRCLE ( 'NONE', #13257, 0.1000000000000002554 ) ;
#4485 = CARTESIAN_POINT ( 'NONE',  ( 0.4465819873849480870, -2.886751345948518566, -5.000000000000000000 ) ) ;
#4486 = EDGE_CURVE ( 'NONE', #11996, #3628, #12017, .T. ) ;
#4487 = VERTEX_POINT ( 'NONE', #4186 ) ;
#4488 = TOROIDAL_SURFACE ( 'NONE', #1179, 2.700000000000000622, 0.2000000000000000111 ) ;
#4489 = AXIS2_PLACEMENT_3D ( 'NONE', #13991, #2527, #6157 ) ;
#4490 = CARTESIAN_POINT ( 'NONE',  ( 6.196878017913831194, -5.292377467571574456, 0.8333333333333328152 ) ) ;
#4491 = ORIENTED_EDGE ( 'NONE', *, *, #430, .F. ) ;
#4492 = ORIENTED_EDGE ( 'NONE', *, *, #2581, .F. ) ;
#4494 = CARTESIAN_POINT ( 'NONE',  ( -6.500000000000000000, 3.752776749732564809, -6.064240316920399110 ) ) ;
#4493 = AXIS2_PLACEMENT_3D ( 'NONE', #9082, #120, #1329 ) ;
#4495 = EDGE_CURVE ( 'NONE', #6201, #2146, #8810, .T. ) ;
#4496 = CIRCLE ( 'NONE', #1184, 4.799999999999968736 ) ;
#4497 = ADVANCED_FACE ( 'NONE', ( #4477 ), #9909, .T. ) ;
#4498 = FACE_OUTER_BOUND ( 'NONE', #62, .T. ) ;
#4500 = VECTOR ( 'NONE', #2295, 1000.000000000000000 ) ;
#4499 = CARTESIAN_POINT ( 'NONE',  ( 6.500000000000000888, 0.000000000000000000, 0.000000000000000000 ) ) ;
#4501 = EDGE_CURVE ( 'NONE', #13831, #5068, #7311, .T. ) ;
#4502 = CONICAL_SURFACE ( 'NONE', #13920, 5.560781378645573980, 1.221730476396046816 ) ;
#4503 = PRODUCT_RELATED_PRODUCT_CATEGORY ( 'part', '', ( #12895 ) ) ;
#4504 = LINE ( 'NONE', #1249, #7585 ) ;
#4505 = CARTESIAN_POINT ( 'NONE',  ( 148.9991633467111569, 386.6211705227183870, 210.0000000000000000 ) ) ;
#4506 = CARTESIAN_POINT ( 'NONE',  ( -2.595115354961444076, -7.673029147243174641, 0.000000000000000000 ) ) ;
#4507 = AXIS2_PLACEMENT_3D ( 'NONE', #8487, #5171, #9596 ) ;
#4508 = CARTESIAN_POINT ( 'NONE',  ( 101.4713065522757063, 338.2376885075856876, 169.9999999999999716 ) ) ;
#4509 = VERTEX_POINT ( 'NONE', #9863 ) ;
#4510 = CIRCLE ( 'NONE', #12036, 5.000000000000004441 ) ;
#4511 = DIRECTION ( 'NONE',  ( 0.000000000000000000, 0.000000000000000000, -1.000000000000000000 ) ) ;
#4512 = CARTESIAN_POINT ( 'NONE',  ( 6.534533895392296898, -5.902695350657469753, 2.508608540288783656E-15 ) ) ;
#4513 = PRODUCT_CONTEXT ( 'NONE', #11586, 'mechanical' ) ;
#4514 = AXIS2_PLACEMENT_3D ( 'NONE', #710, #11779, #5303 ) ;
#4515 = FACE_BOUND ( 'NONE', #6586, .T. ) ;
#4516 =( BOUNDED_SURFACE ( )  B_SPLINE_SURFACE ( 3, 2, ( 
 ( #10982, #5377, #9877 ),
 ( #13281, #3172, #7675 ),
 ( #12157, #2040, #6559 ),
 ( #7949, #8097, #12444 ),
 ( #6767, #12530, #10311 ),
 ( #1464, #1309, #5670 ) ),
 .UNSPECIFIED., .F., .F., .F. ) 
 B_SPLINE_SURFACE_WITH_KNOTS ( ( 4, 2, 4 ),
 ( 3, 3 ),
 ( 0.003190620565844226857, 0.007281897438794493645, 0.01137317431174476000 ),
 ( 0.000000000000000000, 1.000000000000000000 ),
 .UNSPECIFIED. ) 
 GEOMETRIC_REPRESENTATION_ITEM ( )  RATIONAL_B_SPLINE_SURFACE ( (
 ( 1.000000000000000000, 0.8047731410850399447, 1.000000000000000000),
 ( 1.000000000000000000, 0.8125552299147021929, 1.000000000000000000),
 ( 1.000000000000000000, 0.8191520442902128218, 1.000000000000000000),
 ( 1.000000000000000000, 0.8191520442877616714, 1.000000000000000000),
 ( 1.000000000000000000, 0.8125552299165426096, 1.000000000000000000),
 ( 1.000000000000000000, 0.8047731410850402778, 1.000000000000000000) ) ) 
 REPRESENTATION_ITEM ( '' )  SURFACE ( )  );
#4517 = VERTEX_POINT ( 'NONE', #14370 ) ;
#4518 = VERTEX_POINT ( 'NONE', #4264 ) ;
#4519 =( NAMED_UNIT ( * ) SI_UNIT ( $, .STERADIAN. ) SOLID_ANGLE_UNIT ( ) );
#4520 = FACE_OUTER_BOUND ( 'NONE', #1347, .T. ) ;
#4521 = CARTESIAN_POINT ( 'NONE',  ( 639.0000000000000000, 164.0000000000000000, -225.5000000000000000 ) ) ;
#4522 = CIRCLE ( 'NONE', #8991, 2.396904916527700102 ) ;
#4523 = VECTOR ( 'NONE', #8951, 1000.000000000000000 ) ;
#4524 = B_SPLINE_SURFACE_WITH_KNOTS ( 'NONE', 1, 3, ( 
 ( #11703, #2785, #10471, #1601, #629, #7149, #7286, #14019, #333, #9361 ),
 ( #3758, #8244, #7217, #12757, #1534, #9437, #410, #8390, #1686, #13946 ),
 ( #5153, #6115, #6193, #10691, #5087, #9583, #3975, #7368, #9659, #11125 ),
 ( #14299, #13057, #7507, #1006, #14373, #10913, #5237, #8773, #4269, #7590 ) ),
 .UNSPECIFIED., .F., .F., .F.,
 ( 2, 1, 1, 2 ),
 ( 4, 2, 2, 2, 4 ),
 ( -0.01000000000000000021, 0.000000000000000000, 1.000000000000000000, 1.010099999999999998 ),
 ( 0.000000000000000000, 0.2500000000000000000, 0.5000000000000000000, 0.7500000000000000000, 1.000000000000000000 ),
 .UNSPECIFIED. ) ;
#4525 = CARTESIAN_POINT ( 'NONE',  ( 639.0000000000000000, 156.0000000000000000, -233.5000000000000000 ) ) ;
#4526 = DIRECTION ( 'NONE',  ( -1.000000000000000000, 0.000000000000000000, 0.000000000000000000 ) ) ;
#4527 = VERTEX_POINT ( 'NONE', #12144 ) ;
#4528 = ADVANCED_FACE ( 'NONE', ( #6544 ), #7067, .T. ) ;
#4529 = CARTESIAN_POINT ( 'NONE',  ( 6.244297270353402318, 0.9889575675955702971, -5.105276777067857097 ) ) ;
#4530 = DIRECTION ( 'NONE',  ( 0.000000000000000000, 1.000000000000000000, 0.000000000000000000 ) ) ;
#4531 = SURFACE_SIDE_STYLE ('',( #133 ) ) ;
#4532 = AXIS2_PLACEMENT_3D ( 'NONE', #9850, #9784, #8670 ) ;
#4533 = ADVANCED_FACE ( 'NONE', ( #4339 ), #5442, .T. ) ;
#4534 = CARTESIAN_POINT ( 'NONE',  ( 6.355324643801636419, -1.972141403783273850, 5.108685331087992942 ) ) ;
#4535 = EDGE_LOOP ( 'NONE', ( #7873, #11476, #8879, #14354 ) ) ;
#4536 = ORIENTED_EDGE ( 'NONE', *, *, #1667, .T. ) ;
#4537 = CARTESIAN_POINT ( 'NONE',  ( 451.3035746174797396, 294.6698471414878782, 210.0000000000000000 ) ) ;
#4538 =( REPRESENTATION_RELATIONSHIP ('NONE','NONE', #2822, #3781 ) REPRESENTATION_RELATIONSHIP_WITH_TRANSFORMATION ( #9144 )SHAPE_REPRESENTATION_RELATIONSHIP( ) );
#4539 = PRESENTATION_LAYER_ASSIGNMENT (  '', '', ( #9948 ) ) ;
#4540 = DIRECTION ( 'NONE',  ( 0.2873478855663502141, 0.9578262852211498757, -4.382459307730876264E-15 ) ) ;
#4541 = CYLINDRICAL_SURFACE ( 'NONE', #6152, 6.975000000000000533 ) ;
#4542 = EDGE_LOOP ( 'NONE', ( #13166, #13165, #13082 ) ) ;
#4543 = EDGE_CURVE ( 'NONE', #2701, #14449, #1362, .T. ) ;
#4544 = ORIENTED_EDGE ( 'NONE', *, *, #6735, .T. ) ;
#4545 = PLANE ( 'NONE',  #8052 ) ;
#4546 = DIRECTION ( 'NONE',  ( 0.000000000000000000, 0.000000000000000000, 1.000000000000000000 ) ) ;
#4547 = CARTESIAN_POINT ( 'NONE',  ( 6.495567275914605254, 5.834887664330116408, -1.517037228251972982E-15 ) ) ;
#4548 = PLANE ( 'NONE',  #3250 ) ;
#4549 = CARTESIAN_POINT ( 'NONE',  ( 455.5035746174796714, 294.6698471414878782, 210.0000000000000000 ) ) ;
#4550 = EDGE_LOOP ( 'NONE', ( #11695, #10277, #4470, #11035 ) ) ;
#4551 = CARTESIAN_POINT ( 'NONE',  ( 8.500000000000000000, -2.886751345948134873, -5.000000000000000000 ) ) ;
#4552 = VERTEX_POINT ( 'NONE', #13551 ) ;
#4553 = ORIENTED_EDGE ( 'NONE', *, *, #4147, .F. ) ;
#4554 = PRESENTATION_LAYER_ASSIGNMENT (  '', '', ( #2898 ) ) ;
#4555 = FACE_BOUND ( 'NONE', #11560, .T. ) ;
#4556 = ORIENTED_EDGE ( 'NONE', *, *, #547, .T. ) ;
#4557 = SHAPE_REPRESENTATION_RELATIONSHIP ( 'NONE' , 'NONE' ,  #1780, #4558 ) ;
#4558 = ADVANCED_BREP_SHAPE_REPRESENTATION ( '', ( #12340, #9440 ), #13250 ) ;
#4559 = FACE_OUTER_BOUND ( 'NONE', #12030, .T. ) ;
#4560 = ADVANCED_FACE ( 'NONE', ( #11468 ), #11548, .T. ) ;
#4561 = EDGE_CURVE ( 'NONE', #6968, #11364, #9683, .T. ) ;
#4562 = DIRECTION ( 'NONE',  ( -1.000000000000000000, 0.000000000000000000, 0.000000000000000000 ) ) ;
#4563 = AXIS2_PLACEMENT_3D ( 'NONE', #9183, #9106, #11245 ) ;
#4564 = ORIENTED_EDGE ( 'NONE', *, *, #10973, .T. ) ;
#4565 = CARTESIAN_POINT ( 'NONE',  ( 446.3084422793565409, 264.0194060144110608, 190.0000000000000000 ) ) ;
#4566 = LINE ( 'NONE', #3521, #4946 ) ;
#4567 = CARTESIAN_POINT ( 'NONE',  ( -4.197393957002303999, -0.8151795401431414234, -3.503767560748935139 ) ) ;
#4568 =( NAMED_UNIT ( * ) PLANE_ANGLE_UNIT ( ) SI_UNIT ( $, .RADIAN. ) );
#4569 = ORIENTED_EDGE ( 'NONE', *, *, #11840, .T. ) ;
#4570 = DIRECTION ( 'NONE',  ( 1.000000000000000000, 0.000000000000000000, 0.000000000000000000 ) ) ;
#4571 = VERTEX_POINT ( 'NONE', #9274 ) ;
#4572 = ORIENTED_EDGE ( 'NONE', *, *, #2560, .F. ) ;
#4573 = FACE_OUTER_BOUND ( 'NONE', #7783, .T. ) ;
#4574 = CYLINDRICAL_SURFACE ( 'NONE', #11524, 5.525000000000000355 ) ;
#4575 = EDGE_CURVE ( 'NONE', #5821, #6071, #703, .T. ) ;
#4576 = DIRECTION ( 'NONE',  ( 2.022127743178574844E-16, 3.939404418192334771E-15, 1.000000000000000000 ) ) ;
#4577 = DIRECTION ( 'NONE',  ( 9.794481010665704304E-16, 3.264827003555234768E-15, -1.000000000000000000 ) ) ;
#4578 = ADVANCED_FACE ( 'NONE', ( #4559 ), #10136, .T. ) ;
#4579 = DIRECTION ( 'NONE',  ( -0.2873478855663453291, -0.9578262852211513190, 3.835990623682899812E-15 ) ) ;
#4580 = CARTESIAN_POINT ( 'NONE',  ( 639.0000000000000000, 164.0000000000000000, -233.5000000000000000 ) ) ;
#4581 = CARTESIAN_POINT ( 'NONE',  ( 229.2257385731836621, 308.4724102386199434, 179.7999999999995850 ) ) ;
#4582 = VERTEX_POINT ( 'NONE', #3438 ) ;
#4583 = EDGE_CURVE ( 'NONE', #8326, #11698, #10372, .T. ) ;
#4584 = DIRECTION ( 'NONE',  ( -0.000000000000000000, 0.000000000000000000, -1.000000000000000000 ) ) ;
#4585 = CARTESIAN_POINT ( 'NONE',  ( 707.0389973793288618, 162.8315651648156575, -149.9999999999986642 ) ) ;
#4586 = CARTESIAN_POINT ( 'NONE',  ( 6.518095160332177507, -5.866179305614763528, -5.948047347825906810E-16 ) ) ;
#4587 = APPLICATION_PROTOCOL_DEFINITION ( 'draft international standard', 'automotive_design', 1998, #10364 ) ;
#4588 = ORIENTED_EDGE ( 'NONE', *, *, #5783, .T. ) ;
#4590 = EDGE_CURVE ( 'NONE', #783, #12163, #12733, .T. ) ;
#4589 = FACE_OUTER_BOUND ( 'NONE', #1695, .T. ) ;
#4591 = ORIENTED_EDGE ( 'NONE', *, *, #7, .F. ) ;
#4592 = ORIENTED_EDGE ( 'NONE', *, *, #12142, .F. ) ;
#4593 = CARTESIAN_POINT ( 'NONE',  ( 4.024499207728847949, -2.323545700935699454, -3.572172305156873673 ) ) ;
#4594 = DIRECTION ( 'NONE',  ( 0.2873478855663437748, 0.9578262852211518741, 0.000000000000000000 ) ) ;
#4595 = EDGE_CURVE ( 'NONE', #10717, #7536, #9195, .T. ) ;
#4596 = DIRECTION ( 'NONE',  ( -1.000000000000000000, 0.000000000000000000, 0.000000000000000000 ) ) ;
#4597 = DIRECTION ( 'NONE',  ( -6.938893903907222067E-15, 1.000000000000000000, 0.000000000000000000 ) ) ;
#4598 = UNCERTAINTY_MEASURE_WITH_UNIT (LENGTH_MEASURE( 1.000000000000000082E-05 ), #14243, 'distance_accuracy_value', 'NONE');
#4599 = CARTESIAN_POINT ( 'NONE',  ( 6.506891779418575439, -2.833891091414765029, -5.091556646552820808 ) ) ;
#4600 = ORIENTED_EDGE ( 'NONE', *, *, #13694, .F. ) ;
#4601 = ADVANCED_FACE ( 'NONE', ( #12587 ), #13773, .F. ) ;
#4602 = EDGE_CURVE ( 'NONE', #12967, #796, #11315, .T. ) ;
#4603 =( BOUNDED_SURFACE ( )  B_SPLINE_SURFACE ( 3, 2, ( 
 ( #8248, #11708, #4944 ),
 ( #11573, #2492, #2789 ),
 ( #5026, #6993, #14022 ),
 ( #568, #10694, #9295 ),
 ( #2653, #1537, #10621 ),
 ( #12761, #1692, #13798 ) ),
 .UNSPECIFIED., .F., .F., .T. ) 
 B_SPLINE_SURFACE_WITH_KNOTS ( ( 4, 2, 4 ),
 ( 3, 3 ),
 ( 0.02032853247518126225, 0.02278863295364821212, 0.02524873343211516200 ),
 ( 0.000000000000000000, 1.000000000000000000 ),
 .UNSPECIFIED. ) 
 GEOMETRIC_REPRESENTATION_ITEM ( )  RATIONAL_B_SPLINE_SURFACE ( (
 ( 1.000000000000000000, 0.8047781615896835161, 1.000000000000000000),
 ( 1.000000000000000000, 0.8123767586291043008, 1.000000000000000000),
 ( 1.000000000000000000, 0.8190662415562011134, 1.000000000000000000),
 ( 1.000000000000000000, 0.8192361015671398849, 1.000000000000000000),
 ( 1.000000000000000000, 0.8126135807102121689, 1.000000000000000000),
 ( 1.000000000000000000, 0.8047712338318585568, 1.000000000000000000) ) ) 
 REPRESENTATION_ITEM ( '' )  SURFACE ( )  );
#4604 = PLANE ( 'NONE',  #7505 ) ;
#4605 = CARTESIAN_POINT ( 'NONE',  ( 446.3084422793565409, 264.0194060144110608, 187.0000000000000000 ) ) ;
#4607 = EDGE_CURVE ( 'NONE', #3125, #10404, #4784, .T. ) ;
#4606 = CARTESIAN_POINT ( 'NONE',  ( 636.9746078850427011, 155.6249658629529620, 210.0000000000000000 ) ) ;
#4608 = ORIENTED_EDGE ( 'NONE', *, *, #12867, .T. ) ;
#4609 = VERTEX_POINT ( 'NONE', #1224 ) ;
#4610 = CARTESIAN_POINT ( 'NONE',  ( -2.805705207896067144, 3.226868319750155312, -3.503898532754364581 ) ) ;
#4611 = CYLINDRICAL_SURFACE ( 'NONE', #14358, 2.500000000000000444 ) ;
#4612 = DIRECTION ( 'NONE',  ( 1.000000000000000000, 0.000000000000000000, 0.000000000000000000 ) ) ;
#4613 = ORIENTED_EDGE ( 'NONE', *, *, #2412, .F. ) ;
#4614 = VERTEX_POINT ( 'NONE', #13836 ) ;
#4615 = CARTESIAN_POINT ( 'NONE',  ( 635.0000000000000000, 160.0000000000000284, -225.5000000000000000 ) ) ;
#4616 = LINE ( 'NONE', #9103, #13671 ) ;
#4617 = CARTESIAN_POINT ( 'NONE',  ( -4.175648173966055587, 2.207990556236529844, -3.469390959564062626 ) ) ;
#4618 = DIRECTION ( 'NONE',  ( 0.000000000000000000, 0.000000000000000000, -1.000000000000000000 ) ) ;
#4619 = LINE ( 'NONE', #8885, #776 ) ;
#4620 = FILL_AREA_STYLE ('',( #3285 ) ) ;
#4621 = ORIENTED_EDGE ( 'NONE', *, *, #6573, .T. ) ;
#4622 = DIRECTION ( 'NONE',  ( -1.000000000000000000, 0.000000000000000000, 0.000000000000000000 ) ) ;
#4623 = ORIENTED_EDGE ( 'NONE', *, *, #12410, .F. ) ;
#4624 = ORIENTED_EDGE ( 'NONE', *, *, #9717, .T. ) ;
#4625 = DIRECTION ( 'NONE',  ( 0.000000000000000000, 0.000000000000000000, 1.000000000000000000 ) ) ;
#4626 = ORIENTED_EDGE ( 'NONE', *, *, #5299, .T. ) ;
#4627 = DIRECTION ( 'NONE',  ( -0.2873478855663454401, -0.9578262852211514300, 0.000000000000000000 ) ) ;
#4628 = DIRECTION ( 'NONE',  ( 0.000000000000000000, 0.000000000000000000, 1.000000000000000000 ) ) ;
#4629 = ORIENTED_EDGE ( 'NONE', *, *, #14209, .T. ) ;
#4630 = CARTESIAN_POINT ( 'NONE',  ( 6.244297270355323448, 0.4917101305082346441, 5.105276777067912164 ) ) ;
#4631 = LINE ( 'NONE', #5733, #8226 ) ;
#4632 = LINE ( 'NONE', #8016, #7473 ) ;
#4633 = CYLINDRICAL_SURFACE ( 'NONE', #13983, 2.649999999999985700 ) ;
#4634 =( NAMED_UNIT ( * ) SI_UNIT ( $, .STERADIAN. ) SOLID_ANGLE_UNIT ( ) );
#4635 = ORIENTED_EDGE ( 'NONE', *, *, #9010, .T. ) ;
#4636 = CARTESIAN_POINT ( 'NONE',  ( 6.367873360227559232, -5.773502691896264416, 0.000000000000000000 ) ) ;
#4637 = B_SPLINE_CURVE_WITH_KNOTS ( 'NONE', 3,
 ( #10501, #3807, #11457, #454, #7116, #5851, #228, #4772, #8134, #9259 ),
 .UNSPECIFIED., .F., .F.,
 ( 4, 2, 2, 2, 4 ),
 ( 0.000000000000000000, 0.001989602278884365291, 0.003979204557768730582, 0.005968806836653095874, 0.007958409115537461165 ),
 .UNSPECIFIED. ) ;
#4638 = VERTEX_POINT ( 'NONE', #2542 ) ;
#4639 = EDGE_CURVE ( 'NONE', #9573, #4953, #9206, .T. ) ;
#4640 = ORIENTED_EDGE ( 'NONE', *, *, #1413, .F. ) ;
#4641 = CARTESIAN_POINT ( 'NONE',  ( 627.2408731339805854, 284.9098836221799615, -187.0000000000001990 ) ) ;
#4642 = CARTESIAN_POINT ( 'NONE',  ( 0.000000000000000000, 0.000000000000000000, 7.000000000000000000 ) ) ;
#4643 = DIRECTION ( 'NONE',  ( 0.000000000000000000, 0.000000000000000000, -1.000000000000000000 ) ) ;
#4644 = FACE_OUTER_BOUND ( 'NONE', #12280, .T. ) ;
#4645 = DIRECTION ( 'NONE',  ( -0.000000000000000000, -0.000000000000000000, 1.000000000000000000 ) ) ;
#4646 = CARTESIAN_POINT ( 'NONE',  ( 635.0000000000000000, 160.0000000000000284, -211.0000000000000000 ) ) ;
#4647 = LINE ( 'NONE', #4508, #2552 ) ;
#4648 = VERTEX_POINT ( 'NONE', #9116 ) ;
#4649 = DIRECTION ( 'NONE',  ( -0.000000000000000000, -0.000000000000000000, 1.000000000000000000 ) ) ;
#4650 = DIRECTION ( 'NONE',  ( 0.9578262852211507639, -0.2873478855663477716, -0.000000000000000000 ) ) ;
#4651 = CARTESIAN_POINT ( 'NONE',  ( -0.1481481481481481122, -4.797713218419819903, -1.000000000000000000 ) ) ;
#4652 = CONTEXT_DEPENDENT_SHAPE_REPRESENTATION ( #4819, #8294 ) ;
#4653 = EDGE_LOOP ( 'NONE', ( #3954, #5802, #11817, #1355 ) ) ;
#4654 = ADVANCED_FACE ( 'NONE', ( #13619 ), #10453, .F. ) ;
#4655 = FACE_OUTER_BOUND ( 'NONE', #4170, .T. ) ;
#4656 = ORIENTED_EDGE ( 'NONE', *, *, #11917, .T. ) ;
#4657 = EDGE_LOOP ( 'NONE', ( #12040, #4624 ) ) ;
#4658 = PRESENTATION_STYLE_ASSIGNMENT (( #119 ) ) ;
#4659 = B_SPLINE_CURVE_WITH_KNOTS ( 'NONE', 3,
 ( #13072, #2955, #11937, #8263, #4206, #5529 ),
 .UNSPECIFIED., .F., .F.,
 ( 4, 2, 4 ),
 ( -3.640115492409406142E-06, 0.0002066546034003385283, 0.0004169493222930864334 ),
 .UNSPECIFIED. ) ;
#4660 = CARTESIAN_POINT ( 'NONE',  ( 635.0000000000000000, 160.0000000000000284, 215.5000000000000000 ) ) ;
#4661 = AXIS2_PLACEMENT_3D ( 'NONE', #1336, #12398, #131 ) ;
#4663 = CARTESIAN_POINT ( 'NONE',  ( -6.500000000000000000, -3.752776749732572803, -6.064240316920399998 ) ) ;
#4662 = CIRCLE ( 'NONE', #5361, 4.799999999999968736 ) ;
#4664 = ADVANCED_FACE ( 'NONE', ( #8010 ), #3736, .T. ) ;
#4665 = CONICAL_SURFACE ( 'NONE', #7724, 5.000000000000000888, 1.047197551196600296 ) ;
#4666 = CARTESIAN_POINT ( 'NONE',  ( 2.500000000000000000, -2.357898499370432166, 3.035766082959412415E-15 ) ) ;
#4667 = EDGE_CURVE ( 'NONE', #1859, #4684, #10295, .T. ) ;
#4668 = DIRECTION ( 'NONE',  ( 1.000000000000000000, 9.498873539028489960E-17, 0.000000000000000000 ) ) ;
#4669 = EDGE_LOOP ( 'NONE', ( #2744, #3547 ) ) ;
#4670 = B_SPLINE_CURVE_WITH_KNOTS ( 'NONE', 3,
 ( #11195, #9282, #13557, #170, #4711, #2326 ),
 .UNSPECIFIED., .F., .F.,
 ( 4, 2, 4 ),
 ( 0.002365888236227967761, 0.003551327329835077609, 0.004736766423442186590 ),
 .UNSPECIFIED. ) ;
#4671 = AXIS2_PLACEMENT_3D ( 'NONE', #11397, #12578, #149 ) ;
#4672 = FACE_OUTER_BOUND ( 'NONE', #2209, .T. ) ;
#4673 = CARTESIAN_POINT ( 'NONE',  ( -3.309651814758565180, -5.455921364805393026, -1.000000000000000000 ) ) ;
#4674 = CARTESIAN_POINT ( 'NONE',  ( 0.000000000000000000, 0.000000000000000000, -233.5000000000000000 ) ) ;
#4675 = ORIENTED_EDGE ( 'NONE', *, *, #4232, .F. ) ;
#4676 = ORIENTED_EDGE ( 'NONE', *, *, #4639, .F. ) ;
#4677 = LINE ( 'NONE', #7022, #382 ) ;
#4678 = CYLINDRICAL_SURFACE ( 'NONE', #10883, 5.750000000000000000 ) ;
#4679 = LINE ( 'NONE', #8067, #8460 ) ;
#4680 = AXIS2_PLACEMENT_3D ( 'NONE', #3552, #9235, #10414 ) ;
#4681 = EDGE_CURVE ( 'NONE', #1630, #11949, #4999, .T. ) ;
#4682 = CARTESIAN_POINT ( 'NONE',  ( 4.000000000000000888, 0.8228435280416209752, -3.430609588141487976 ) ) ;
#4683 = AXIS2_PLACEMENT_3D ( 'NONE', #13828, #1434, #10286 ) ;
#4684 = VERTEX_POINT ( 'NONE', #9714 ) ;
#4685 = ADVANCED_FACE ( 'NONE', ( #684 ), #5209, .F. ) ;
#4686 = PRODUCT_RELATED_PRODUCT_CATEGORY ( 'part', '', ( #2394 ) ) ;
#4687 = EDGE_LOOP ( 'NONE', ( #6124, #4771, #1948, #10936, #7758, #8433, #1308, #13323 ) ) ;
#4688 = DIRECTION ( 'NONE',  ( 1.000000000000000000, 0.000000000000000000, 0.000000000000000000 ) ) ;
#4689 = CARTESIAN_POINT ( 'NONE',  ( 702.5260191523640287, 164.1854586329053518, 177.6000000000001648 ) ) ;
#4690 = PLANE ( 'NONE',  #11724 ) ;
#4691 = DIRECTION ( 'NONE',  ( -0.000000000000000000, -0.000000000000000000, 1.000000000000000000 ) ) ;
#4692 = CARTESIAN_POINT ( 'NONE',  ( -4.000000000000000000, 4.898587196589412829E-16, -8.000000000000000000 ) ) ;
#4693 = ORIENTED_EDGE ( 'NONE', *, *, #8621, .T. ) ;
#4694 = VECTOR ( 'NONE', #2951, 1000.000000000000000 ) ;
#4695 = FACE_OUTER_BOUND ( 'NONE', #1984, .T. ) ;
#4696 = AXIS2_PLACEMENT_3D ( 'NONE', #4605, #13667, #11381 ) ;
#4697 = AXIS2_PLACEMENT_3D ( 'NONE', #13351, #8791, #13217 ) ;
#4698 = VERTEX_POINT ( 'NONE', #6304 ) ;
#4699 = ORIENTED_EDGE ( 'NONE', *, *, #13587, .F. ) ;
#4700 = FACE_BOUND ( 'NONE', #13236, .T. ) ;
#4701 = AXIS2_PLACEMENT_3D ( 'NONE', #6932, #11577, #12455 ) ;
#4702 = B_SPLINE_CURVE_WITH_KNOTS ( 'NONE', 3,
 ( #2389, #6605, #12349, #6, #2085, #10284 ),
 .UNSPECIFIED., .F., .F.,
 ( 4, 2, 4 ),
 ( 0.003841072314098346787, 0.005765657563962181195, 0.007690242813826015170 ),
 .UNSPECIFIED. ) ;
#4703 = DIRECTION ( 'NONE',  ( 0.000000000000000000, 0.000000000000000000, 1.000000000000000000 ) ) ;
#4704 = CARTESIAN_POINT ( 'NONE',  ( 0.000000000000000000, -1.178949249685214307, 2.042000000000001592 ) ) ;
#4705 = AXIS2_PLACEMENT_3D ( 'NONE', #12713, #6148, #8353 ) ;
#4706 = AXIS2_PLACEMENT_3D ( 'NONE', #5259, #13076, #2961 ) ;
#4707 = ORIENTED_EDGE ( 'NONE', *, *, #10439, .F. ) ;
#4708 = DIRECTION ( 'NONE',  ( 1.000000000000000000, 0.000000000000000000, 0.000000000000000000 ) ) ;
#4709 = DIRECTION ( 'NONE',  ( -1.000000000000000000, 0.000000000000000000, 0.000000000000000000 ) ) ;
#4710 = DIRECTION ( 'NONE',  ( -0.000000000000000000, -0.000000000000000000, 1.000000000000000000 ) ) ;
#4711 = CARTESIAN_POINT ( 'NONE',  ( 0.3208286057739604957, -4.433571671609698228, -0.3503314178412692548 ) ) ;
#4712 = ORIENTED_EDGE ( 'NONE', *, *, #8221, .T. ) ;
#4713 = AXIS2_PLACEMENT_3D ( 'NONE', #5011, #11852, #1527 ) ;
#4714 = EDGE_CURVE ( 'NONE', #8605, #13901, #10672, .T. ) ;
#4715 = CARTESIAN_POINT ( 'NONE',  ( 642.0000000000000000, 235.0000000000000284, -225.5000000000000000 ) ) ;
#4716 = EDGE_LOOP ( 'NONE', ( #7226, #9896, #9589, #7453 ) ) ;
#4717 = VECTOR ( 'NONE', #13742, 1000.000000000000000 ) ;
#4718 = ADVANCED_FACE ( 'NONE', ( #9565 ), #2843, .F. ) ;
#4719 = CIRCLE ( 'NONE', #11998, 20.00000000000001776 ) ;
#4720 = ORIENTED_EDGE ( 'NONE', *, *, #1326, .T. ) ;
#4721 = CARTESIAN_POINT ( 'NONE',  ( 705.2654023280961155, 165.6605111121464518, 177.6000000000000512 ) ) ;
#4722 = CARTESIAN_POINT ( 'NONE',  ( 634.0059381729540746, 152.5000994061731490, -210.0000000000000000 ) ) ;
#4723 = VECTOR ( 'NONE', #3199, 1000.000000000000114 ) ;
#4724 = CARTESIAN_POINT ( 'NONE',  ( 610.0000000000000000, 10.00000000000005507, -210.0020000000000095 ) ) ;
#4725 = EDGE_LOOP ( 'NONE', ( #5446, #12549 ) ) ;
#4726 = DIRECTION ( 'NONE',  ( 0.9578262852211514300, -0.2873478855663454956, 0.000000000000000000 ) ) ;
#4727 = CIRCLE ( 'NONE', #4961, 2.199999999999757705 ) ;
#4728 = VECTOR ( 'NONE', #2616, 1000.000000000000114 ) ;
#4729 = EDGE_CURVE ( 'NONE', #12823, #5137, #11905, .T. ) ;
#4730 = CARTESIAN_POINT ( 'NONE',  ( 0.03421028094652913548, -3.855830693249139962, -1.321505333908958413 ) ) ;
#4731 = FACE_OUTER_BOUND ( 'NONE', #4220, .T. ) ;
#4732 = DIRECTION ( 'NONE',  ( 0.000000000000000000, 0.000000000000000000, -1.000000000000000000 ) ) ;
#4733 = VERTEX_POINT ( 'NONE', #4030 ) ;
#4734 = FACE_OUTER_BOUND ( 'NONE', #1990, .T. ) ;
#4735 = CARTESIAN_POINT ( 'NONE',  ( 1.250000000000000000, -6.429618962271402616, 0.000000000000000000 ) ) ;
#4736 = DIRECTION ( 'NONE',  ( 1.000000000000000000, 0.000000000000000000, 0.000000000000000000 ) ) ;
#4737 = ORIENTED_EDGE ( 'NONE', *, *, #12037, .T. ) ;
#4738 = VECTOR ( 'NONE', #12771, 1000.000000000000000 ) ;
#4739 = AXIS2_PLACEMENT_3D ( 'NONE', #11947, #2899, #4082 ) ;
#4740 = CARTESIAN_POINT ( 'NONE',  ( 448.9584422793565750, 264.0194060144110608, 187.0000000000000000 ) ) ;
#4741 = ORIENTED_EDGE ( 'NONE', *, *, #11904, .T. ) ;
#4742 = EDGE_LOOP ( 'NONE', ( #6867, #12768, #6697, #10922, #11115, #6041, #12911, #3480, #1186, #14101, #12099, #6702 ) ) ;
#4743 =( LENGTH_UNIT ( ) NAMED_UNIT ( * ) SI_UNIT ( .MILLI., .METRE. ) );
#4744 = DIRECTION ( 'NONE',  ( 0.000000000000000000, 0.000000000000000000, 1.000000000000000000 ) ) ;
#4745 = AXIS2_PLACEMENT_3D ( 'NONE', #471, #5071, #3950 ) ;
#4746 = AXIS2_PLACEMENT_3D ( 'NONE', #9554, #1725, #11964 ) ;
#4747 = CARTESIAN_POINT ( 'NONE',  ( 6.403457969954073903, -2.888443235695458355, 5.002930439003193896 ) ) ;
#4748 = AXIS2_PLACEMENT_3D ( 'NONE', #10484, #14099, #12848 ) ;
#4749 = EDGE_CURVE ( 'NONE', #13126, #4582, #6088, .T. ) ;
#4750 = CARTESIAN_POINT ( 'NONE',  ( 2.500000000000000000, 2.357898499370431722, -2.818925648462311528E-15 ) ) ;
#4751 = AXIS2_PLACEMENT_3D ( 'NONE', #12075, #11994, #1891 ) ;
#4752 = UNCERTAINTY_MEASURE_WITH_UNIT (LENGTH_MEASURE( 1.000000000000000082E-05 ), #12400, 'distance_accuracy_value', 'NONE');
#4753 = CARTESIAN_POINT ( 'NONE',  ( 6.362374563308424769, -3.415000007735117027, -4.302769906043429238 ) ) ;
#4754 = ORIENTED_EDGE ( 'NONE', *, *, #3576, .T. ) ;
#4755 = AXIS2_PLACEMENT_3D ( 'NONE', #6496, #7606, #8483 ) ;
#4756 = CARTESIAN_POINT ( 'NONE',  ( 631.0000000000000000, 155.9999999999999432, -233.5000000000000000 ) ) ;
#4757 = CARTESIAN_POINT ( 'NONE',  ( 639.0000000000000000, 164.0000000000000000, -233.5000000000000000 ) ) ;
#4758 = CARTESIAN_POINT ( 'NONE',  ( 0.000000000000000000, 0.000000000000000000, 0.000000000000000000 ) ) ;
#4759 = PLANE ( 'NONE',  #6385 ) ;
#4760 = ORIENTED_EDGE ( 'NONE', *, *, #6017, .T. ) ;
#4761 = ORIENTED_EDGE ( 'NONE', *, *, #2474, .T. ) ;
#4762 = AXIS2_PLACEMENT_3D ( 'NONE', #12210, #8549, #1816 ) ;
#4763 = CARTESIAN_POINT ( 'NONE',  ( 642.5000000000002274, 159.0182522957532569, 210.0000120000000265 ) ) ;
#4764 = DIRECTION ( 'NONE',  ( 2.022127743178574844E-16, 3.939404418192334771E-15, -1.000000000000000000 ) ) ;
#4765 = LINE ( 'NONE', #3799, #7763 ) ;
#4766 = AXIS2_PLACEMENT_3D ( 'NONE', #11919, #5085, #6112 ) ;
#4767 = MECHANICAL_DESIGN_GEOMETRIC_PRESENTATION_REPRESENTATION (  '', ( #6170 ), #7109 ) ;
#4768 = EDGE_CURVE ( 'NONE', #10480, #3223, #1516, .T. ) ;
#4769 = EDGE_LOOP ( 'NONE', ( #11308, #11042, #7080, #978, #5555 ) ) ;
#4770 = VECTOR ( 'NONE', #7424, 1000.000000000000000 ) ;
#4771 = ORIENTED_EDGE ( 'NONE', *, *, #8135, .F. ) ;
#4772 = CARTESIAN_POINT ( 'NONE',  ( 1.126429428730187032, -7.232124035235040438, -6.344710093416088270 ) ) ;
#4773 = CARTESIAN_POINT ( 'NONE',  ( -4.236525694536558362, 2.416953475386465211, -3.751298745799836354 ) ) ;
#4774 = CARTESIAN_POINT ( 'NONE',  ( -8.505790995055050985, 376.6597771564184995, 184.8000000000000398 ) ) ;
#4775 = SURFACE_STYLE_USAGE ( .BOTH. , #232 ) ;
#4776 = EDGE_CURVE ( 'NONE', #2271, #7181, #10513, .T. ) ;
#4777 = ORIENTED_EDGE ( 'NONE', *, *, #1295, .T. ) ;
#4778 = EDGE_CURVE ( 'NONE', #2837, #13718, #2120, .T. ) ;
#4779 = LINE ( 'NONE', #9109, #1174 ) ;
#4780 = ORIENTED_EDGE ( 'NONE', *, *, #2429, .T. ) ;
#4781 = VERTEX_POINT ( 'NONE', #13923 ) ;
#4782 = CARTESIAN_POINT ( 'NONE',  ( 0.000000000000000000, 0.000000000000000000, -190.0000000000000000 ) ) ;
#4783 = EDGE_CURVE ( 'NONE', #1364, #11582, #2841, .T. ) ;
#4784 = LINE ( 'NONE', #9341, #14165 ) ;
#4785 = DIRECTION ( 'NONE',  ( -0.2873478855663502141, -0.9578262852211498757, 3.895519384649669193E-15 ) ) ;
#4786 = AXIS2_PLACEMENT_3D ( 'NONE', #12499, #7557, #65 ) ;
#4787 = ORIENTED_EDGE ( 'NONE', *, *, #9384, .F. ) ;
#4788 = DIRECTION ( 'NONE',  ( -0.000000000000000000, -0.000000000000000000, -1.000000000000000000 ) ) ;
#4789 = CARTESIAN_POINT ( 'NONE',  ( 10.00000000000000000, 0.000000000000000000, 190.0000000000000000 ) ) ;
#4790 = CARTESIAN_POINT ( 'NONE',  ( -1.274258131565027874, -3.883108878240886241, -3.220599429844051009 ) ) ;
#4791 = FILL_AREA_STYLE_COLOUR ( '', #485 ) ;
#4792 = AXIS2_PLACEMENT_3D ( 'NONE', #3444, #7943, #10087 ) ;
#4793 = ORIENTED_EDGE ( 'NONE', *, *, #14141, .T. ) ;
#4794 = EDGE_CURVE ( 'NONE', #9268, #14518, #9496, .T. ) ;
#4795 = ADVANCED_FACE ( 'NONE', ( #3889 ), #7343, .T. ) ;
#4796 = CARTESIAN_POINT ( 'NONE',  ( -8.505790995055013681, 418.4210031920606525, 187.0000000000000000 ) ) ;
#4797 = ORIENTED_EDGE ( 'NONE', *, *, #7269, .F. ) ;
#4798 = CARTESIAN_POINT ( 'NONE',  ( -20.63749999999999929, 6.766173565289127388E-16, 5.525000000000000355 ) ) ;
#4799 = EDGE_LOOP ( 'NONE', ( #539, #13382, #5109, #1583 ) ) ;
#4800 = DIRECTION ( 'NONE',  ( 0.000000000000000000, 0.000000000000000000, 1.000000000000000000 ) ) ;
#4801 = CARTESIAN_POINT ( 'NONE',  ( -4.211140560182196957, 2.431303136016537803, -3.745885042887433514 ) ) ;
#4802 = PLANE ( 'NONE',  #11798 ) ;
#4803 = EDGE_CURVE ( 'NONE', #3508, #13279, #469, .T. ) ;
#4804 = EDGE_LOOP ( 'NONE', ( #3380, #13487 ) ) ;
#4805 = DIRECTION ( 'NONE',  ( 0.000000000000000000, 0.000000000000000000, 1.000000000000000000 ) ) ;
#4806 = ADVANCED_FACE ( 'NONE', ( #12879, #2761 ), #6237, .T. ) ;
#4807 = CARTESIAN_POINT ( 'NONE',  ( 112.9652219749295341, 376.5507399164317803, -210.0000000000000000 ) ) ;
#4808 = DIRECTION ( 'NONE',  ( 0.000000000000000000, 0.000000000000000000, -1.000000000000000000 ) ) ;
#4809 = CARTESIAN_POINT ( 'NONE',  ( 107.2182642636026202, 357.3942142120087055, -190.0000000000000000 ) ) ;
#4810 = EDGE_LOOP ( 'NONE', ( #13970, #11199 ) ) ;
#4811 = CARTESIAN_POINT ( 'NONE',  ( 610.8620436566989156, 230.3137853645732775, 184.7999999999999829 ) ) ;
#4812 = CARTESIAN_POINT ( 'NONE',  ( 0.000000000000000000, -4.330127018922194537, -2.500000000000000444 ) ) ;
#4813 = EDGE_LOOP ( 'NONE', ( #3694, #877 ) ) ;
#4814 = DIRECTION ( 'NONE',  ( 0.000000000000000000, 0.000000000000000000, -1.000000000000000000 ) ) ;
#4815 = ORIENTED_EDGE ( 'NONE', *, *, #942, .F. ) ;
#4816 = ORIENTED_EDGE ( 'NONE', *, *, #12241, .T. ) ;
#4817 = DIRECTION ( 'NONE',  ( -0.2873478855663434972, -0.9578262852211520961, 0.000000000000000000 ) ) ;
#4818 = CARTESIAN_POINT ( 'NONE',  ( 2.500000000000000000, 2.357898499370431722, -2.818925648462311528E-15 ) ) ;
#4819 =( REPRESENTATION_RELATIONSHIP ('NONE','NONE', #2822, #6959 ) REPRESENTATION_RELATIONSHIP_WITH_TRANSFORMATION ( #6935 )SHAPE_REPRESENTATION_RELATIONSHIP( ) );
#4820 = DIRECTION ( 'NONE',  ( 0.000000000000000000, 0.000000000000000000, 1.000000000000000000 ) ) ;
#4821 = LINE ( 'NONE', #9381, #6730 ) ;
#4822 = VERTEX_POINT ( 'NONE', #11755 ) ;
#4823 = CARTESIAN_POINT ( 'NONE',  ( -2.141486166123589996, 6.269165884987821791, -0.07763482564820804732 ) ) ;
#4824 = CARTESIAN_POINT ( 'NONE',  ( -2.688821387764050996E-14, -4.618802153517012954, -0.4999999999999995559 ) ) ;
#4825 = DIRECTION ( 'NONE',  ( 1.000000000000000000, 0.000000000000000000, 0.000000000000000000 ) ) ;
#4826 = LINE ( 'NONE', #7018, #9201 ) ;
#4827 = ORIENTED_EDGE ( 'NONE', *, *, #5484, .F. ) ;
#4828 = ORIENTED_EDGE ( 'NONE', *, *, #3510, .T. ) ;
#4829 = CARTESIAN_POINT ( 'NONE',  ( 628.4466020873429670, 156.2228576472182056, 210.0000119999999981 ) ) ;
#4830 = FACE_OUTER_BOUND ( 'NONE', #7515, .T. ) ;
#4831 = ADVANCED_FACE ( 'NONE', ( #6171 ), #4488, .F. ) ;
#4832 = CARTESIAN_POINT ( 'NONE',  ( 6.207530437345011087, 3.810448612249821565, 3.400109403952575882 ) ) ;
#4833 = EDGE_LOOP ( 'NONE', ( #12191, #3897, #5199, #9320 ) ) ;
#4834 = ORIENTED_EDGE ( 'NONE', *, *, #4089, .F. ) ;
#4835 = CARTESIAN_POINT ( 'NONE',  ( 610.7375075899259400, 188.5899201489639267, -185.0880224589102454 ) ) ;
#4836 = PLANE ( 'NONE',  #9429 ) ;
#4837 = CARTESIAN_POINT ( 'NONE',  ( 6.534838248920899595, 5.903531555104835071, -2.091255385257999292E-17 ) ) ;
#4838 = LINE ( 'NONE', #536, #2801 ) ;
#4839 = CARTESIAN_POINT ( 'NONE',  ( -0.5620262070071414540, 7.564407249984292037, -6.443844059477446429 ) ) ;
#4840 =( LENGTH_UNIT ( ) NAMED_UNIT ( * ) SI_UNIT ( .MILLI., .METRE. ) );
#4841 = AXIS2_PLACEMENT_3D ( 'NONE', #6431, #10771, #13213 ) ;
#4842 = ORIENTED_EDGE ( 'NONE', *, *, #11654, .T. ) ;
#4843 = CARTESIAN_POINT ( 'NONE',  ( 1.257172072275274388, -3.892973519170983110, -3.433252694550781303 ) ) ;
#4844 = ORIENTED_EDGE ( 'NONE', *, *, #3123, .T. ) ;
#4845 = ORIENTED_EDGE ( 'NONE', *, *, #13136, .F. ) ;
#4846 = DIRECTION ( 'NONE',  ( -0.000000000000000000, -0.000000000000000000, 1.000000000000000000 ) ) ;
#4847 = EDGE_CURVE ( 'NONE', #5524, #10447, #8525, .T. ) ;
#4848 = EDGE_CURVE ( 'NONE', #8553, #1030, #2080, .T. ) ;
#4849 = CARTESIAN_POINT ( 'NONE',  ( 1.400000000000001910, 0.000000000000000000, 0.000000000000000000 ) ) ;
#4850 = CARTESIAN_POINT ( 'NONE',  ( 3.339999999999998970, 0.000000000000000000, -0.4621369752184044666 ) ) ;
#4852 = EDGE_CURVE ( 'NONE', #4518, #10329, #223, .T. ) ;
#4851 = CARTESIAN_POINT ( 'NONE',  ( 4.197393957002303999, 7.772902908466098641E-14, -3.503767560748929810 ) ) ;
#4853 = ORIENTED_EDGE ( 'NONE', *, *, #2748, .T. ) ;
#4854 = CARTESIAN_POINT ( 'NONE',  ( 4.211140560182196957, 2.431303136016536470, -3.745885042887433514 ) ) ;
#4855 = CARTESIAN_POINT ( 'NONE',  ( 6.500000000000001776, -4.012858516023013244, -6.470130706010830401 ) ) ;
#4856 = EDGE_CURVE ( 'NONE', #7551, #5805, #5500, .T. ) ;
#4857 = CARTESIAN_POINT ( 'NONE',  ( 6.371506350351444858, -3.439339428956428080, 4.260454149911180544 ) ) ;
#4858 = CARTESIAN_POINT ( 'NONE',  ( 237.7887055630605744, 337.0156335382089310, -182.8000000000007219 ) ) ;
#4859 = ORIENTED_EDGE ( 'NONE', *, *, #11310, .F. ) ;
#4860 = SURFACE_STYLE_FILL_AREA ( #557 ) ;
#4861 = VERTEX_POINT ( 'NONE', #5558 ) ;
#4862 = AXIS2_PLACEMENT_3D ( 'NONE', #4887, #351, #13811 ) ;
#4863 = VERTEX_POINT ( 'NONE', #5346 ) ;
#4864 = FACE_BOUND ( 'NONE', #99, .T. ) ;
#4865 = DIRECTION ( 'NONE',  ( 1.148424442117023040E-15, -3.445273326351216045E-16, -1.000000000000000000 ) ) ;
#4866 = ADVANCED_FACE ( 'NONE', ( #11173 ), #5284, .F. ) ;
#4867 = PLANE ( 'NONE',  #2370 ) ;
#4868 = EDGE_CURVE ( 'NONE', #10150, #8680, #4028, .T. ) ;
#4869 = ORIENTED_EDGE ( 'NONE', *, *, #4923, .F. ) ;
#4870 = CARTESIAN_POINT ( 'NONE',  ( 0.1983443223721602366, -5.300482436767283367, -0.8192951148925881055 ) ) ;
#4871 = EDGE_CURVE ( 'NONE', #4433, #10237, #10890, .T. ) ;
#4872 = DIRECTION ( 'NONE',  ( -0.000000000000000000, -0.000000000000000000, 1.000000000000000000 ) ) ;
#4873 = CARTESIAN_POINT ( 'NONE',  ( 6.499999999999997335, 1.286902272306391870, -0.09436334093186085625 ) ) ;
#4874 = CARTESIAN_POINT ( 'NONE',  ( 0.1973348417602838190, -1.936114729415324920, -5.000000000000000000 ) ) ;
#4875 = ORIENTED_EDGE ( 'NONE', *, *, #10891, .T. ) ;
#4876 = PLANE ( 'NONE',  #4701 ) ;
#4877 = DIRECTION ( 'NONE',  ( -1.000000000000000000, -7.930164461608254918E-15, 0.000000000000000000 ) ) ;
#4878 = ORIENTED_EDGE ( 'NONE', *, *, #10443, .F. ) ;
#4879 = DIRECTION ( 'NONE',  ( -0.2873478855663477161, -0.9578262852211506528, 1.261617073437870380E-13 ) ) ;
#4880 = ORIENTED_EDGE ( 'NONE', *, *, #1526, .T. ) ;
#4881 = VERTEX_POINT ( 'NONE', #12269 ) ;
#4882 = CARTESIAN_POINT ( 'NONE',  ( 708.1388811837596222, 164.7984674554459446, -149.9999999999986642 ) ) ;
#4883 = CARTESIAN_POINT ( 'NONE',  ( 4.999999999999997335, 5.204748896376250699E-16, -4.250000000000000000 ) ) ;
#4884 = CARTESIAN_POINT ( 'NONE',  ( 6.420058897733096792, -2.891482565094588342, 5.008194711943423805 ) ) ;
#4885 = CARTESIAN_POINT ( 'NONE',  ( 0.1920286436967153787, 0.000000000000000000, 0.000000000000000000 ) ) ;
#4886 = UNCERTAINTY_MEASURE_WITH_UNIT (LENGTH_MEASURE( 1.000000000000000082E-05 ), #12067, 'distance_accuracy_value', 'NONE');
#4887 = CARTESIAN_POINT ( 'NONE',  ( 0.2500000000000002220, 0.000000000000000000, 0.000000000000000000 ) ) ;
#4888 = ORIENTED_EDGE ( 'NONE', *, *, #2307, .F. ) ;
#4889 = CARTESIAN_POINT ( 'NONE',  ( 0.08165819712376926054, 4.939961795957294122, 1.443735181952768620 ) ) ;
#4890 = FACE_OUTER_BOUND ( 'NONE', #11371, .T. ) ;
#4891 = CARTESIAN_POINT ( 'NONE',  ( 0.000000000000000000, 0.000000000000000000, 0.000000000000000000 ) ) ;
#4892 = CIRCLE ( 'NONE', #380, 5.199999999999760369 ) ;
#4893 = FACE_OUTER_BOUND ( 'NONE', #3769, .T. ) ;
#4894 = AXIS2_PLACEMENT_3D ( 'NONE', #5134, #14135, #3952 ) ;
#4895 = VERTEX_POINT ( 'NONE', #767 ) ;
#4896 = ORIENTED_EDGE ( 'NONE', *, *, #13115, .T. ) ;
#4897 = CARTESIAN_POINT ( 'NONE',  ( 639.6091003998118367, 154.0024986820136235, 210.0000119999999981 ) ) ;
#4898 = CARTESIAN_POINT ( 'NONE',  ( 650.0000000000000000, 175.0000000000000568, -190.0000000000000000 ) ) ;
#4899 = DIRECTION ( 'NONE',  ( -1.000000000000000000, 0.000000000000000000, 0.000000000000000000 ) ) ;
#4901 = ORIENTED_EDGE ( 'NONE', *, *, #6531, .F. ) ;
#4900 = MECHANICAL_DESIGN_GEOMETRIC_PRESENTATION_REPRESENTATION (  '', ( #1105 ), #13143 ) ;
#4902 = VECTOR ( 'NONE', #6314, 1000.000000000000114 ) ;
#4903 = LINE ( 'NONE', #3805, #12093 ) ;
#4904 = DIRECTION ( 'NONE',  ( 1.000000000000000000, 0.000000000000000000, -0.000000000000000000 ) ) ;
#4905 = EDGE_CURVE ( 'NONE', #9542, #11993, #14351, .T. ) ;
#4906 = LINE ( 'NONE', #13905, #4962 ) ;
#4907 = EDGE_CURVE ( 'NONE', #30, #12192, #13171, .T. ) ;
#4908 = CARTESIAN_POINT ( 'NONE',  ( 0.03363697881402896717, -0.7786124122131675707, -4.000000000000000000 ) ) ;
#4909 = CYLINDRICAL_SURFACE ( 'NONE', #4432, 4.000000000000000000 ) ;
#4910 = FACE_OUTER_BOUND ( 'NONE', #1063, .T. ) ;
#4911 = ORIENTED_EDGE ( 'NONE', *, *, #4130, .T. ) ;
#4912 = DIRECTION ( 'NONE',  ( 0.000000000000000000, 0.000000000000000000, 1.000000000000000000 ) ) ;
#4913 = ORIENTED_EDGE ( 'NONE', *, *, #10628, .T. ) ;
#4914 = ORIENTED_EDGE ( 'NONE', *, *, #14113, .T. ) ;
#4915 = CARTESIAN_POINT ( 'NONE',  ( 610.8620436566991430, 188.5525593289318920, 184.8000000000000682 ) ) ;
#4916 = CIRCLE ( 'NONE', #7028, 4.000000000000000000 ) ;
#4917 = DIRECTION ( 'NONE',  ( -6.938893903907222067E-15, 1.000000000000000000, 0.000000000000000000 ) ) ;
#4918 =( REPRESENTATION_RELATIONSHIP ('NONE','NONE', #2822, #1780 ) REPRESENTATION_RELATIONSHIP_WITH_TRANSFORMATION ( #12072 )SHAPE_REPRESENTATION_RELATIONSHIP( ) );
#4919 = DIRECTION ( 'NONE',  ( -1.000000000000000000, -0.000000000000000000, -0.000000000000000000 ) ) ;
#4920 = DIRECTION ( 'NONE',  ( 0.000000000000000000, 0.000000000000000000, 1.000000000000000000 ) ) ;
#4921 = ORIENTED_EDGE ( 'NONE', *, *, #9878, .F. ) ;
#4922 = DIRECTION ( 'NONE',  ( -0.2873478855663454401, -0.9578262852211514300, -4.197634718856730240E-17 ) ) ;
#4923 = EDGE_CURVE ( 'NONE', #238, #2880, #4980, .T. ) ;
#4924 = CARTESIAN_POINT ( 'NONE',  ( 708.1388811837591675, 164.7984674554467119, 177.5999999999999091 ) ) ;
#4925 = AXIS2_PLACEMENT_3D ( 'NONE', #2335, #1377, #10392 ) ;
#4926 = AXIS2_PLACEMENT_3D ( 'NONE', #3483, #3264, #4377 ) ;
#4927 = CARTESIAN_POINT ( 'NONE',  ( 650.0000000000000000, 145.0000000000000568, 190.0000000000000000 ) ) ;
#4928 = DIRECTION ( 'NONE',  ( 0.9578262852211513190, -0.2873478855663453846, 0.000000000000000000 ) ) ;
#4929 = EDGE_LOOP ( 'NONE', ( #343, #9489, #650, #5904 ) ) ;
#4930 = FACE_OUTER_BOUND ( 'NONE', #1890, .T. ) ;
#4931 = VERTEX_POINT ( 'NONE', #2162 ) ;
#4932 = EDGE_CURVE ( 'NONE', #809, #5257, #2610, .T. ) ;
#4933 = PLANE ( 'NONE',  #12944 ) ;
#4934 = AXIS2_PLACEMENT_3D ( 'NONE', #12860, #9173, #13899 ) ;
#4935 = CARTESIAN_POINT ( 'NONE',  ( 640.0000000000000000, 160.0000000000000284, 187.5000000000000000 ) ) ;
#4936 = DIRECTION ( 'NONE',  ( -0.000000000000000000, -0.000000000000000000, 1.000000000000000000 ) ) ;
#4937 = B_SPLINE_CURVE_WITH_KNOTS ( 'NONE', 3,
 ( #4196, #13125, #1825, #8557, #8623, #13063, #1908, #6421, #10921, #3093 ),
 .UNSPECIFIED., .F., .F.,
 ( 4, 2, 2, 2, 4 ),
 ( 0.009353627468483380336, 0.01031000219096067302, 0.01126637691343796571, 0.01222275163591525840, 0.01317912635839255109 ),
 .UNSPECIFIED. ) ;
#4938 = EDGE_LOOP ( 'NONE', ( #4780, #1928, #2571, #3912 ) ) ;
#4939 = CARTESIAN_POINT ( 'NONE',  ( 0.4465819873852049926, -5.773502691896264416, 5.911082023588295771E-17 ) ) ;
#4940 = EDGE_CURVE ( 'NONE', #11405, #4156, #1900, .T. ) ;
#4941 = PRESENTATION_LAYER_ASSIGNMENT (  '', '', ( #7761 ) ) ;
#4942 = DIRECTION ( 'NONE',  ( -1.000000000000000000, 0.000000000000000000, 0.000000000000000000 ) ) ;
#4943 = CARTESIAN_POINT ( 'NONE',  ( 2.500000000000000000, -2.357898499370432166, 3.035766082959412415E-15 ) ) ;
#4944 = CARTESIAN_POINT ( 'NONE',  ( 4.235886605889389145, 2.417314728048528760, -3.751161874094018245 ) ) ;
#4945 = ORIENTED_EDGE ( 'NONE', *, *, #12312, .F. ) ;
#4946 = VECTOR ( 'NONE', #2105, 1000.000000000000114 ) ;
#4947 =( NAMED_UNIT ( * ) PLANE_ANGLE_UNIT ( ) SI_UNIT ( $, .RADIAN. ) );
#4948 = CARTESIAN_POINT ( 'NONE',  ( 610.0000000000000000, 0.000000000000000000, -210.0000000000000000 ) ) ;
#4949 = ORIENTED_EDGE ( 'NONE', *, *, #13390, .T. ) ;
#4950 = EDGE_CURVE ( 'NONE', #14014, #10129, #9926, .T. ) ;
#4951 = EDGE_CURVE ( 'NONE', #1897, #2224, #2134, .T. ) ;
#4952 = CARTESIAN_POINT ( 'NONE',  ( 6.323290364501794159, 2.010128762266915725, 4.999999999999998224 ) ) ;
#4953 = VERTEX_POINT ( 'NONE', #1875 ) ;
#4954 = ORIENTED_EDGE ( 'NONE', *, *, #9632, .F. ) ;
#4955 = DIRECTION ( 'NONE',  ( -0.8660254037844382635, -0.5000000000000006661, 0.000000000000000000 ) ) ;
#4956 = FACE_OUTER_BOUND ( 'NONE', #6783, .T. ) ;
#4957 = CIRCLE ( 'NONE', #12951, 5.000000000000004441 ) ;
#4958 = EDGE_CURVE ( 'NONE', #12373, #14148, #13252, .T. ) ;
#4959 = DIRECTION ( 'NONE',  ( 1.000000000000000000, 0.000000000000000000, 0.000000000000000000 ) ) ;
#4961 = AXIS2_PLACEMENT_3D ( 'NONE', #3754, #5746, #2484 ) ;
#4960 = DIRECTION ( 'NONE',  ( -0.000000000000000000, -0.000000000000000000, 1.000000000000000000 ) ) ;
#4962 = VECTOR ( 'NONE', #10576, 1000.000000000000000 ) ;
#4963 = DIRECTION ( 'NONE',  ( 1.000000000000000000, 9.498873539028489960E-17, 0.000000000000000000 ) ) ;
#4964 = CARTESIAN_POINT ( 'NONE',  ( 1.500000000000001332, 0.000000000000000000, -5.525000000000000355 ) ) ;
#4965 = ORIENTED_EDGE ( 'NONE', *, *, #4602, .T. ) ;
#4966 = TOROIDAL_SURFACE ( 'NONE', #13207, 4.000000000000000000, 0.2500000000000000000 ) ;
#4967 = DIRECTION ( 'NONE',  ( 0.000000000000000000, -1.000000000000000000, 0.000000000000000000 ) ) ;
#4968 = CARTESIAN_POINT ( 'NONE',  ( -9.999999999999957367, 376.8992337277236970, 190.0000000000000000 ) ) ;
#4969 = DIRECTION ( 'NONE',  ( 1.000000000000000000, 0.000000000000000000, 0.000000000000000000 ) ) ;
#4970 = AXIS2_PLACEMENT_3D ( 'NONE', #5794, #5728, #7044 ) ;
#4971 = DIRECTION ( 'NONE',  ( 0.000000000000000000, -1.000000000000000000, 0.000000000000000000 ) ) ;
#4972 = VECTOR ( 'NONE', #10473, 1000.000000000000114 ) ;
#4973 = ORIENTED_EDGE ( 'NONE', *, *, #1532, .F. ) ;
#4974 = ORIENTED_EDGE ( 'NONE', *, *, #4475, .T. ) ;
#4975 = CARTESIAN_POINT ( 'NONE',  ( 4.000000000000000000, -2.309401076758514915, -3.433295621305383349 ) ) ;
#4976 = CARTESIAN_POINT ( 'NONE',  ( -10.00000000000000000, 413.4403065089105667, -187.0000000000000000 ) ) ;
#4977 = LINE ( 'NONE', #13757, #3269 ) ;
#4978 = CIRCLE ( 'NONE', #13216, 4.199999999999981526 ) ;
#4979 = PLANE ( 'NONE',  #8473 ) ;
#4980 = CIRCLE ( 'NONE', #7092, 7.000000000000000000 ) ;
#4981 = VERTEX_POINT ( 'NONE', #3205 ) ;
#4982 = EDGE_CURVE ( 'NONE', #2440, #5056, #578, .T. ) ;
#4983 = DIRECTION ( 'NONE',  ( -0.9578262852211514300, 0.2873478855663454401, 0.000000000000000000 ) ) ;
#4984 = FACE_OUTER_BOUND ( 'NONE', #11870, .T. ) ;
#4985 = LINE ( 'NONE', #3655, #12979 ) ;
#4986 = ADVANCED_FACE ( 'NONE', ( #900 ), #7619, .F. ) ;
#4987 = FACE_OUTER_BOUND ( 'NONE', #11240, .T. ) ;
#4988 = DIRECTION ( 'NONE',  ( -0.2873478855663446629, -0.9578262852211516520, 5.337610695313252962E-15 ) ) ;
#4989 = DIRECTION ( 'NONE',  ( 0.000000000000000000, 0.000000000000000000, -1.000000000000000000 ) ) ;
#4990 = AXIS2_PLACEMENT_3D ( 'NONE', #13298, #7845, #3046 ) ;
#4991 = VERTEX_POINT ( 'NONE', #7230 ) ;
#4992 = VECTOR ( 'NONE', #10479, 1000.000000000000000 ) ;
#4993 = DIRECTION ( 'NONE',  ( 1.000000000000000000, 0.000000000000000000, 0.000000000000000000 ) ) ;
#4994 = ORIENTED_EDGE ( 'NONE', *, *, #8209, .F. ) ;
#4995 = ORIENTED_EDGE ( 'NONE', *, *, #8442, .T. ) ;
#4996 = CARTESIAN_POINT ( 'NONE',  ( 610.0000000000002274, 185.6790804732676747, -8.443403382996446544E-13 ) ) ;
#4997 = AXIS2_PLACEMENT_3D ( 'NONE', #7878, #10160, #12363 ) ;
#4998 = ADVANCED_FACE ( 'NONE', ( #10281, #9457 ), #3358, .F. ) ;
#4999 = LINE ( 'NONE', #14217, #12731 ) ;
#5000 = VECTOR ( 'NONE', #11782, 1000.000000000000114 ) ;
#5001 = VECTOR ( 'NONE', #6147, 1000.000000000000000 ) ;
#5002 = B_SPLINE_CURVE_WITH_KNOTS ( 'NONE', 3,
 ( #3394, #11275, #5527, #4418, #8918, #9067, #13565, #4285 ),
 .UNSPECIFIED., .F., .F.,
 ( 4, 2, 2, 4 ),
 ( 0.000000000000000000, 0.002450665683189819262, 0.003675998524784728893, 0.004901331366379639391 ),
 .UNSPECIFIED. ) ;
#5003 = CARTESIAN_POINT ( 'NONE',  ( 142.4540310085880606, 355.9707293956415697, 210.0000000000000000 ) ) ;
#5004 = DIRECTION ( 'NONE',  ( -0.2873478855662898734, -0.9578262852211680833, 0.000000000000000000 ) ) ;
#5005 = ORIENTED_EDGE ( 'NONE', *, *, #11131, .F. ) ;
#5006 = CARTESIAN_POINT ( 'NONE',  ( 2.449848172108560096, 3.432307619358740514, -3.503702292528905637 ) ) ;
#5007 = PLANE ( 'NONE',  #4247 ) ;
#5008 = CARTESIAN_POINT ( 'NONE',  ( -4.140404888673278272, -2.228338276487456415, -3.686887068327035166 ) ) ;
#5009 = PRESENTATION_STYLE_ASSIGNMENT (( #1588 ) ) ;
#5010 = EDGE_LOOP ( 'NONE', ( #1398, #3487, #13533, #12472 ) ) ;
#5011 = CARTESIAN_POINT ( 'NONE',  ( 0.000000000000000000, 0.000000000000000000, 190.0000000000000000 ) ) ;
#5012 = DIRECTION ( 'NONE',  ( -0.9578262852211514300, 0.2873478855663454401, 0.000000000000000000 ) ) ;
#5013 = ADVANCED_FACE ( 'NONE', ( #1619 ), #4541, .F. ) ;
#5014 = EDGE_LOOP ( 'NONE', ( #8276, #11969, #5300, #9186 ) ) ;
#5015 = CIRCLE ( 'NONE', #1929, 5.000000000000004441 ) ;
#5016 = CARTESIAN_POINT ( 'NONE',  ( 4.024499207728848837, 2.323545700935681246, -3.572172305156870564 ) ) ;
#5017 = ADVANCED_FACE ( 'NONE', ( #10135 ), #3579, .F. ) ;
#5018 = AXIS2_PLACEMENT_3D ( 'NONE', #12564, #8273, #13815 ) ;
#5019 = DIRECTION ( 'NONE',  ( 1.000000000000000000, 0.000000000000000000, 0.000000000000000000 ) ) ;
#5020 = CARTESIAN_POINT ( 'NONE',  ( 590.0000000000000000, 0.000000000000000000, -210.0000000000000000 ) ) ;
#5021 = AXIS2_PLACEMENT_3D ( 'NONE', #1535, #13947, #10619 ) ;
#5022 = EDGE_LOOP ( 'NONE', ( #2399, #11250, #6023, #11449 ) ) ;
#5023 = DIRECTION ( 'NONE',  ( -0.000000000000000000, -0.000000000000000000, 1.000000000000000000 ) ) ;
#5024 = DIRECTION ( 'NONE',  ( 1.000000000000000000, 0.000000000000000000, 0.000000000000000000 ) ) ;
#5025 = CARTESIAN_POINT ( 'NONE',  ( 6.500000000000000000, 3.149025070564758888, -0.5705737632551094451 ) ) ;
#5026 = CARTESIAN_POINT ( 'NONE',  ( 2.756197834950227410, 3.027510591568626896, -3.223146290109805356 ) ) ;
#5027 = ORIENTED_EDGE ( 'NONE', *, *, #4907, .F. ) ;
#5028 = SURFACE_STYLE_USAGE ( .BOTH. , #7222 ) ;
#5029 = ORIENTED_EDGE ( 'NONE', *, *, #8532, .F. ) ;
#5030 = CARTESIAN_POINT ( 'NONE',  ( 3.700000000000000178, 3.306546357697854226E-16, 2.700000000000000622 ) ) ;
#5031 = VERTEX_POINT ( 'NONE', #10214 ) ;
#5032 = AXIS2_PLACEMENT_3D ( 'NONE', #11847, #8449, #9422 ) ;
#5033 = PLANE ( 'NONE',  #3503 ) ;
#5034 = EDGE_CURVE ( 'NONE', #5667, #2108, #8336, .T. ) ;
#5035 = DIRECTION ( 'NONE',  ( 0.000000000000000000, 0.000000000000000000, -1.000000000000000000 ) ) ;
#5036 = EDGE_CURVE ( 'NONE', #11959, #4117, #5867, .T. ) ;
#5037 = DIRECTION ( 'NONE',  ( -1.000000000000000000, -9.498873539028489960E-17, 0.000000000000000000 ) ) ;
#5038 = FACE_OUTER_BOUND ( 'NONE', #12256, .T. ) ;
#5039 = ADVANCED_FACE ( 'NONE', ( #5710 ), #1548, .F. ) ;
#5040 = PRODUCT_DEFINITION_CONTEXT ( 'detailed design', #10844, 'design' ) ;
#5041 = AXIS2_PLACEMENT_3D ( 'NONE', #6315, #4116, #6397 ) ;
#5042 = CARTESIAN_POINT ( 'NONE',  ( 610.0000000000000000, 227.4403065089105951, -190.0000000000000000 ) ) ;
#5043 = ORIENTED_EDGE ( 'NONE', *, *, #7396, .T. ) ;
#5044 = ADVANCED_FACE ( 'NONE', ( #2728 ), #13599, .T. ) ;
#5045 = DIRECTION ( 'NONE',  ( 0.2873478855663470499, 0.9578262852211508749, 0.000000000000000000 ) ) ;
#5046 = CARTESIAN_POINT ( 'NONE',  ( -10.00000000000000000, 413.4403065089105667, 187.0000000000000000 ) ) ;
#5047 = PRODUCT_CONTEXT ( 'NONE', #12826, 'mechanical' ) ;
#5048 = FACE_OUTER_BOUND ( 'NONE', #3309, .T. ) ;
#5049 = ORIENTED_EDGE ( 'NONE', *, *, #11337, .T. ) ;
#5050 = ORIENTED_EDGE ( 'NONE', *, *, #12056, .F. ) ;
#5051 = CARTESIAN_POINT ( 'NONE',  ( 610.0000000000001137, 185.6790804732683853, 169.9999999999999716 ) ) ;
#5052 = CARTESIAN_POINT ( 'NONE',  ( 6.080745460913608902, 0.5192545390863916310, -1.000000000000000000 ) ) ;
#5053 = CARTESIAN_POINT ( 'NONE',  ( -1.500000000000001332, 7.041719095097280880E-16, 5.750000000000000000 ) ) ;
#5054 = FACE_OUTER_BOUND ( 'NONE', #6181, .T. ) ;
#5055 = EDGE_CURVE ( 'NONE', #3065, #9114, #6808, .T. ) ;
#5056 = VERTEX_POINT ( 'NONE', #3855 ) ;
#5057 = ADVANCED_FACE ( 'NONE', ( #2230 ), #14039, .F. ) ;
#5058 = LINE ( 'NONE', #9484, #4095 ) ;
#5059 = DIRECTION ( 'NONE',  ( 0.000000000000000000, 0.000000000000000000, -1.000000000000000000 ) ) ;
#5060 = PLANE ( 'NONE',  #4746 ) ;
#5061 = ADVANCED_FACE ( 'NONE', ( #12916 ), #10985, .F. ) ;
#5062 = CARTESIAN_POINT ( 'NONE',  ( -1.500000000000001332, 0.000000000000000000, -5.750000000000000000 ) ) ;
#5063 = DIRECTION ( 'NONE',  ( -0.000000000000000000, -0.000000000000000000, -1.000000000000000000 ) ) ;
#5064 = PRESENTATION_STYLE_ASSIGNMENT (( #3810 ) ) ;
#5065 = SURFACE_STYLE_FILL_AREA ( #10505 ) ;
#5066 = ORIENTED_EDGE ( 'NONE', *, *, #4446, .F. ) ;
#5067 = CARTESIAN_POINT ( 'NONE',  ( 5.978033218201114884, 4.054134411712192687, -0.5602453477493293255 ) ) ;
#5068 = VERTEX_POINT ( 'NONE', #13132 ) ;
#5069 = ORIENTED_EDGE ( 'NONE', *, *, #2214, .F. ) ;
#5070 = CARTESIAN_POINT ( 'NONE',  ( 631.0000000000000000, 155.9999999999999432, -233.5000000000000000 ) ) ;
#5071 = DIRECTION ( 'NONE',  ( 0.000000000000000000, 0.000000000000000000, -1.000000000000000000 ) ) ;
#5072 = DIRECTION ( 'NONE',  ( 0.000000000000000000, 0.000000000000000000, 1.000000000000000000 ) ) ;
#5073 = CARTESIAN_POINT ( 'NONE',  ( 3.250000000000000444, 5.629165124598851655, -5.592027715088707218 ) ) ;
#5074 = EDGE_LOOP ( 'NONE', ( #10981, #13032, #10388, #8298 ) ) ;
#5075 = FACE_OUTER_BOUND ( 'NONE', #11435, .T. ) ;
#5076 = DIRECTION ( 'NONE',  ( -1.000000000000000000, 0.000000000000000000, -0.000000000000000000 ) ) ;
#5077 = FACE_OUTER_BOUND ( 'NONE', #4550, .T. ) ;
#5078 =( NAMED_UNIT ( * ) SI_UNIT ( $, .STERADIAN. ) SOLID_ANGLE_UNIT ( ) );
#5079 = ORIENTED_EDGE ( 'NONE', *, *, #4321, .F. ) ;
#5080 = CARTESIAN_POINT ( 'NONE',  ( 637.0568832135862749, 155.4426727739092655, -210.0000000000000000 ) ) ;
#5081 = CARTESIAN_POINT ( 'NONE',  ( 6.385552186430389021, 2.886751345948121550, -5.000000000000001776 ) ) ;
#5082 = EDGE_LOOP ( 'NONE', ( #10308, #7471, #13099, #8772 ) ) ;
#5083 = CARTESIAN_POINT ( 'NONE',  ( 6.080745460913608902, 0.5192545390863916310, 0.000000000000000000 ) ) ;
#5084 = CARTESIAN_POINT ( 'NONE',  ( -6.837824896291514243, 3.947820044545427454, -6.564402953523716278 ) ) ;
#5085 = DIRECTION ( 'NONE',  ( 0.9578262852211514300, -0.2873478855663454956, 1.110223024625157329E-15 ) ) ;
#5086 = ORIENTED_EDGE ( 'NONE', *, *, #11506, .F. ) ;
#5087 = CARTESIAN_POINT ( 'NONE',  ( 610.2340919441475080, 189.6262799281293212, 186.5592670532760167 ) ) ;
#5088 = LINE ( 'NONE', #9363, #7840 ) ;
#5089 = DIRECTION ( 'NONE',  ( -1.000000000000000000, -0.000000000000000000, -0.000000000000000000 ) ) ;
#5090 = CARTESIAN_POINT ( 'NONE',  ( 139.8040310085880833, 355.9707293956415697, -210.0000000000000000 ) ) ;
#5091 = EDGE_CURVE ( 'NONE', #5856, #5202, #6852, .T. ) ;
#5092 = VERTEX_POINT ( 'NONE', #2802 ) ;
#5093 = CARTESIAN_POINT ( 'NONE',  ( -4.000000000000000000, -1.680117682357936904, -3.316611593218794951 ) ) ;
#5094 = CARTESIAN_POINT ( 'NONE',  ( -8.505790995054914205, 376.6597771564183859, -187.0000000000000284 ) ) ;
#5095 = ORIENTED_EDGE ( 'NONE', *, *, #13006, .F. ) ;
#5096 =( REPRESENTATION_RELATIONSHIP ('NONE','NONE', #2822, #9980 ) REPRESENTATION_RELATIONSHIP_WITH_TRANSFORMATION ( #3546 )SHAPE_REPRESENTATION_RELATIONSHIP( ) );
#5097 = ORIENTED_EDGE ( 'NONE', *, *, #4501, .F. ) ;
#5098 = CARTESIAN_POINT ( 'NONE',  ( 6.539198257602126141, -3.775407874310924505, -6.286450516131050215 ) ) ;
#5099 = FACE_OUTER_BOUND ( 'NONE', #7075, .T. ) ;
#5100 = CARTESIAN_POINT ( 'NONE',  ( 6.242800618755127928, 3.923709308887747937, -3.414402460853335430 ) ) ;
#5101 = DIRECTION ( 'NONE',  ( 0.000000000000000000, -1.000000000000000000, 0.000000000000000000 ) ) ;
#5102 = CARTESIAN_POINT ( 'NONE',  ( 635.0000000000000000, 160.0000000000000284, -210.0000000000000000 ) ) ;
#5103 = EDGE_CURVE ( 'NONE', #2837, #2855, #13463, .T. ) ;
#5104 = EDGE_LOOP ( 'NONE', ( #1693, #6603, #12360 ) ) ;
#5105 = DIRECTION ( 'NONE',  ( -1.000000000000000000, -0.000000000000000000, -0.000000000000000000 ) ) ;
#5106 = CARTESIAN_POINT ( 'NONE',  ( 145.1678582058265476, 408.6511750828048548, 190.0000000000000000 ) ) ;
#5107 = DIRECTION ( 'NONE',  ( 0.000000000000000000, 0.000000000000000000, 1.000000000000000000 ) ) ;
#5108 = DIRECTION ( 'NONE',  ( 0.9578262852211513190, -0.2873478855663453846, 0.000000000000000000 ) ) ;
#5109 = ORIENTED_EDGE ( 'NONE', *, *, #8864, .F. ) ;
#5110 = EDGE_LOOP ( 'NONE', ( #2177, #4834, #6422, #13887 ) ) ;
#5111 = DIRECTION ( 'NONE',  ( -0.000000000000000000, -0.000000000000000000, -1.000000000000000000 ) ) ;
#5112 = LINE ( 'NONE', #1420, #2632 ) ;
#5113 = EDGE_CURVE ( 'NONE', #10210, #8605, #1832, .T. ) ;
#5114 = FACE_BOUND ( 'NONE', #13576, .T. ) ;
#5115 = CARTESIAN_POINT ( 'NONE',  ( 0.000000000000000000, 0.000000000000000000, 0.000000000000000000 ) ) ;
#5116 = ORIENTED_EDGE ( 'NONE', *, *, #13902, .F. ) ;
#5117 = PLANE ( 'NONE',  #6677 ) ;
#5118 = FACE_OUTER_BOUND ( 'NONE', #2421, .T. ) ;
#5119 = FACE_OUTER_BOUND ( 'NONE', #4177, .T. ) ;
#5120 = EDGE_CURVE ( 'NONE', #2950, #10050, #13071, .T. ) ;
#5121 = DIRECTION ( 'NONE',  ( -1.000000000000000000, -0.000000000000000000, -0.000000000000000000 ) ) ;
#5122 = CARTESIAN_POINT ( 'NONE',  ( 2.100000000000000089, 0.000000000000000000, -4.694516984716113228 ) ) ;
#5123 = CYLINDRICAL_SURFACE ( 'NONE', #13169, 7.500000000000062172 ) ;
#5124 = SURFACE_STYLE_FILL_AREA ( #8809 ) ;
#5125 = VERTEX_POINT ( 'NONE', #2954 ) ;
#5126 = CARTESIAN_POINT ( 'NONE',  ( -4.101948962586059011, 2.368261337751163875, -3.681124513963739187 ) ) ;
#5127 = ORIENTED_EDGE ( 'NONE', *, *, #9254, .T. ) ;
#5128 = VERTEX_POINT ( 'NONE', #728 ) ;
#5129 = CARTESIAN_POINT ( 'NONE',  ( -4.000000000000000000, 0.9868501483902560878, -0.09357334158579519445 ) ) ;
#5130 = EDGE_CURVE ( 'NONE', #9582, #6727, #9674, .T. ) ;
#5131 = VECTOR ( 'NONE', #6123, 1000.000000000000000 ) ;
#5132 = ADVANCED_FACE ( 'NONE', ( #11933 ), #9814, .F. ) ;
#5133 = AXIS2_PLACEMENT_3D ( 'NONE', #8303, #2699, #2763 ) ;
#5134 = CARTESIAN_POINT ( 'NONE',  ( 635.0000000000000000, 160.0000000000000284, 207.0000000000000000 ) ) ;
#5135 = CARTESIAN_POINT ( 'NONE',  ( 635.0000000000000000, 160.0000000000000284, -210.0000000000000000 ) ) ;
#5136 = PRODUCT ( 'handle', 'handle', '', ( #12319 ) ) ;
#5137 = VERTEX_POINT ( 'NONE', #6267 ) ;
#5138 = FACE_OUTER_BOUND ( 'NONE', #1806, .T. ) ;
#5139 = CARTESIAN_POINT ( 'NONE',  ( 636.9631091326946262, 167.3047950750124642, 210.0000119999999981 ) ) ;
#5140 = LINE ( 'NONE', #8531, #4902 ) ;
#5141 = CYLINDRICAL_SURFACE ( 'NONE', #10911, 6.975000000000000533 ) ;
#5142 = ADVANCED_FACE ( 'NONE', ( #9593 ), #9750, .F. ) ;
#5143 = VERTEX_POINT ( 'NONE', #14032 ) ;
#5144 = CIRCLE ( 'NONE', #1597, 7.500000000000062172 ) ;
#5145 = FACE_BOUND ( 'NONE', #2677, .T. ) ;
#5146 = CARTESIAN_POINT ( 'NONE',  ( 610.4899793196105975, 188.8968529749589038, 185.7755421771552165 ) ) ;
#5147 = VERTEX_POINT ( 'NONE', #3918 ) ;
#5148 = FACE_BOUND ( 'NONE', #153, .T. ) ;
#5149 = DIRECTION ( 'NONE',  ( 0.3543563944859323689, -0.9351104457158684324, 0.000000000000000000 ) ) ;
#5150 = CARTESIAN_POINT ( 'NONE',  ( 629.0000000000000000, 154.0000000000000284, -187.5000000000000000 ) ) ;
#5151 = AXIS2_PLACEMENT_3D ( 'NONE', #11966, #3051, #3130 ) ;
#5152 = ORIENTED_EDGE ( 'NONE', *, *, #9828, .T. ) ;
#5153 = CARTESIAN_POINT ( 'NONE',  ( 610.0000000000001137, 191.1080398579019572, 187.0000000000000284 ) ) ;
#5154 = CARTESIAN_POINT ( 'NONE',  ( -8.331345277524542681, 1.020295532671184640E-15, -7.381345277524544279 ) ) ;
#5155 = ADVANCED_FACE ( 'NONE', ( #11802 ), #8402, .F. ) ;
#5156 = CARTESIAN_POINT ( 'NONE',  ( -2.344047193898593395, -3.265465875126480455, -1.054683074273691752E-14 ) ) ;
#5157 = CARTESIAN_POINT ( 'NONE',  ( 33.50000000000000000, 0.000000000000000000, 0.000000000000000000 ) ) ;
#5158 = CARTESIAN_POINT ( 'NONE',  ( -1.243802165048909503, 3.900692638707381921, -3.223146290109805800 ) ) ;
#5159 = ORIENTED_EDGE ( 'NONE', *, *, #5304, .F. ) ;
#5160 = EDGE_CURVE ( 'NONE', #1836, #12898, #2856, .T. ) ;
#5161 = CARTESIAN_POINT ( 'NONE',  ( -4.000000000000000000, -2.472261339043343220, -3.687027428081192326 ) ) ;
#5162 = DIRECTION ( 'NONE',  ( -1.063400795443705011E-15, 3.190202386331112862E-16, 1.000000000000000000 ) ) ;
#5163 = ORIENTED_EDGE ( 'NONE', *, *, #6726, .T. ) ;
#5164 = CONICAL_SURFACE ( 'NONE', #13403, 2.499999999999946709, 1.029744259999984646 ) ;
#5165 = EDGE_LOOP ( 'NONE', ( #10161, #226, #13580, #7884 ) ) ;
#5166 = CARTESIAN_POINT ( 'NONE',  ( 2.500000000000000000, -1.178949249685214307, 2.042000000000001592 ) ) ;
#5167 = LINE ( 'NONE', #8564, #10827 ) ;
#5168 = AXIS2_PLACEMENT_3D ( 'NONE', #2977, #1728, #13023 ) ;
#5169 = DIRECTION ( 'NONE',  ( -1.000000000000000000, -0.000000000000000000, -0.000000000000000000 ) ) ;
#5170 = EDGE_CURVE ( 'NONE', #5125, #10470, #3764, .T. ) ;
#5171 = DIRECTION ( 'NONE',  ( 1.000000000000000000, 0.000000000000000000, 0.000000000000000000 ) ) ;
#5172 = AXIS2_PLACEMENT_3D ( 'NONE', #7890, #7820, #7741 ) ;
#5173 = AXIS2_PLACEMENT_3D ( 'NONE', #3964, #5012, #11429 ) ;
#5174 = DIRECTION ( 'NONE',  ( -1.000000000000000000, 0.000000000000000000, 0.000000000000000000 ) ) ;
#5175 = ORIENTED_EDGE ( 'NONE', *, *, #14089, .T. ) ;
#5176 = CARTESIAN_POINT ( 'NONE',  ( -1.399999999999999689, 0.000000000000000000, -7.399999999999999467 ) ) ;
#5177 = DIRECTION ( 'NONE',  ( 0.9396926207859143121, 1.150791560227857665E-16, -0.3420201433256525592 ) ) ;
#5178 = CARTESIAN_POINT ( 'NONE',  ( 459.7035746174795463, 294.6698471414878782, 190.0000000000000568 ) ) ;
#5179 = ORIENTED_EDGE ( 'NONE', *, *, #4047, .T. ) ;
#5180 = ORIENTED_EDGE ( 'NONE', *, *, #3002, .F. ) ;
#5181 = CYLINDRICAL_SURFACE ( 'NONE', #3972, 5.249999999999976907 ) ;
#5182 = DIRECTION ( 'NONE',  ( -0.9237280213470676626, -0.3830490080632388272, 0.000000000000000000 ) ) ;
#5183 = CIRCLE ( 'NONE', #14369, 0.6186547224754559426 ) ;
#5184 = DIRECTION ( 'NONE',  ( 1.000000000000000000, 0.000000000000000000, -0.000000000000000000 ) ) ;
#5185 = EDGE_CURVE ( 'NONE', #12209, #12104, #3317, .T. ) ;
#5186 = DIRECTION ( 'NONE',  ( 0.000000000000000000, 0.000000000000000000, -1.000000000000000000 ) ) ;
#5187 = TOROIDAL_SURFACE ( 'NONE', #10134, 7.399999999999999467, 0.1000000000000000472 ) ;
#5188 = VERTEX_POINT ( 'NONE', #7743 ) ;
#5189 = DIRECTION ( 'NONE',  ( -0.2873478855663477161, -0.9578262852211506528, 0.000000000000000000 ) ) ;
#5190 = DIRECTION ( 'NONE',  ( 0.000000000000000000, 0.000000000000000000, -1.000000000000000000 ) ) ;
#5191 = DIRECTION ( 'NONE',  ( -1.000000000000000000, -0.000000000000000000, -0.000000000000000000 ) ) ;
#5192 = ORIENTED_EDGE ( 'NONE', *, *, #12792, .F. ) ;
#5193 = CIRCLE ( 'NONE', #8008, 0.7499999999999997780 ) ;
#5194 = VECTOR ( 'NONE', #1054, 1000.000000000000000 ) ;
#5195 = CARTESIAN_POINT ( 'NONE',  ( 0.1578711657514692002, -1.548887424847152694, -4.000000000000000000 ) ) ;
#5196 = CARTESIAN_POINT ( 'NONE',  ( -4.555094537983154446, -5.243183837310248840, -6.208110906918257399 ) ) ;
#5197 = FACE_OUTER_BOUND ( 'NONE', #5165, .T. ) ;
#5198 = SURFACE_STYLE_USAGE ( .BOTH. , #5413 ) ;
#5199 = ORIENTED_EDGE ( 'NONE', *, *, #8812, .T. ) ;
#5200 = CARTESIAN_POINT ( 'NONE',  ( -3.333333333333332149, -2.694301256218264218, -3.300726591567082036 ) ) ;
#5201 = ORIENTED_EDGE ( 'NONE', *, *, #14136, .T. ) ;
#5202 = VERTEX_POINT ( 'NONE', #2340 ) ;
#5203 = CIRCLE ( 'NONE', #475, 2.700000000000000622 ) ;
#5204 = DIRECTION ( 'NONE',  ( 1.000000000000000000, 0.000000000000000000, 0.000000000000000000 ) ) ;
#5205 = AXIS2_PLACEMENT_3D ( 'NONE', #5474, #11289, #11069 ) ;
#5206 = EDGE_CURVE ( 'NONE', #12163, #1716, #2199, .T. ) ;
#5207 = VECTOR ( 'NONE', #20, 1000.000000000000114 ) ;
#5208 = VECTOR ( 'NONE', #1020, 1000.000000000000000 ) ;
#5209 = PLANE ( 'NONE',  #714 ) ;
#5210 = DIRECTION ( 'NONE',  ( -3.469446951953611033E-15, -1.000000000000000000, 0.000000000000000000 ) ) ;
#5211 = EDGE_CURVE ( 'NONE', #3152, #13868, #5592, .T. ) ;
#5212 = VERTEX_POINT ( 'NONE', #11355 ) ;
#5213 = AXIS2_PLACEMENT_3D ( 'NONE', #4750, #5766, #2506 ) ;
#5214 = ORIENTED_EDGE ( 'NONE', *, *, #12240, .T. ) ;
#5215 = EDGE_CURVE ( 'NONE', #8752, #2870, #7822, .T. ) ;
#5216 = DIRECTION ( 'NONE',  ( 1.078061080328271067E-15, 7.457226491206363694E-15, 1.000000000000000000 ) ) ;
#5217 = CARTESIAN_POINT ( 'NONE',  ( 0.000000000000000000, 0.000000000000000000, -4.974599999999998801 ) ) ;
#5218 = CIRCLE ( 'NONE', #235, 4.199999999999981526 ) ;
#5219 = EDGE_CURVE ( 'NONE', #992, #10412, #9038, .T. ) ;
#5220 = CARTESIAN_POINT ( 'NONE',  ( 0.000000000000000000, 0.000000000000000000, -0.3080913168122742518 ) ) ;
#5221 = DIRECTION ( 'NONE',  ( -1.000000000000000000, -0.000000000000000000, -0.000000000000000000 ) ) ;
#5222 =( LENGTH_UNIT ( ) NAMED_UNIT ( * ) SI_UNIT ( .MILLI., .METRE. ) );
#5223 = ORIENTED_EDGE ( 'NONE', *, *, #13922, .F. ) ;
#5224 = VECTOR ( 'NONE', #1117, 1000.000000000000000 ) ;
#5225 = ADVANCED_FACE ( 'NONE', ( #8847 ), #6564, .F. ) ;
#5226 =( GEOMETRIC_REPRESENTATION_CONTEXT ( 3 ) GLOBAL_UNCERTAINTY_ASSIGNED_CONTEXT ( ( #8406 ) ) GLOBAL_UNIT_ASSIGNED_CONTEXT ( ( #1077, #4568, #4634 ) ) REPRESENTATION_CONTEXT ( 'NONE', 'WORKASPACE' ) );
#5227 = LINE ( 'NONE', #6403, #11056 ) ;
#5228 = DIRECTION ( 'NONE',  ( 0.9578262852211513190, -0.2873478855663453291, -0.000000000000000000 ) ) ;
#5229 = ORIENTED_EDGE ( 'NONE', *, *, #5384, .T. ) ;
#5230 = ORIENTED_EDGE ( 'NONE', *, *, #6916, .F. ) ;
#5231 = B_SPLINE_CURVE_WITH_KNOTS ( 'NONE', 3,
 ( #9521, #1386, #9443, #4874, #5892, #10403 ),
 .UNSPECIFIED., .F., .F.,
 ( 4, 2, 4 ),
 ( 0.01799235506992014066, 0.01945319861728520699, 0.02091404216465027679 ),
 .UNSPECIFIED. ) ;
#5232 = VECTOR ( 'NONE', #7066, 999.9999999999998863 ) ;
#5233 = VECTOR ( 'NONE', #2839, 1000.000000000000114 ) ;
#5234 = DIRECTION ( 'NONE',  ( 0.9351104457158685435, 0.3543563944859324244, 0.000000000000000000 ) ) ;
#5235 = CARTESIAN_POINT ( 'NONE',  ( 2.354826896168714434, -6.962563485461402024, -1.000000000000000000 ) ) ;
#5236 = VERTEX_POINT ( 'NONE', #12378 ) ;
#5237 = CARTESIAN_POINT ( 'NONE',  ( 610.4513696044788276, 188.9932989497419555, 185.8927021017107677 ) ) ;
#5238 = CARTESIAN_POINT ( 'NONE',  ( 702.5260191523640287, 164.1854586329053518, -177.6000000000005059 ) ) ;
#5239 = EDGE_CURVE ( 'NONE', #12920, #12815, #7601, .T. ) ;
#5240 = EDGE_CURVE ( 'NONE', #10781, #9509, #11097, .T. ) ;
#5241 = CARTESIAN_POINT ( 'NONE',  ( 448.9584422793565750, 264.0194060144110608, -187.0000000000000000 ) ) ;
#5242 = FILL_AREA_STYLE ('',( #7594 ) ) ;
#5243 = CIRCLE ( 'NONE', #9238, 4.199999999999926459 ) ;
#5244 = ORIENTED_EDGE ( 'NONE', *, *, #2922, .F. ) ;
#5245 = DIRECTION ( 'NONE',  ( -0.9578262852211513190, 0.2873478855663453846, 0.000000000000000000 ) ) ;
#5246 = ORIENTED_EDGE ( 'NONE', *, *, #12791, .F. ) ;
#5247 = AXIS2_PLACEMENT_3D ( 'NONE', #10643, #2449, #12630 ) ;
#5248 = ORIENTED_EDGE ( 'NONE', *, *, #6239, .F. ) ;
#5249 = CARTESIAN_POINT ( 'NONE',  ( 3.700000000000000178, 0.000000000000000000, 2.500000000000000444 ) ) ;
#5250 = EDGE_CURVE ( 'NONE', #8797, #12815, #1296, .T. ) ;
#5251 = CARTESIAN_POINT ( 'NONE',  ( 1.400000000000000133, 0.000000000000000000, -5.100000000000000533 ) ) ;
#5252 = AXIS2_PLACEMENT_3D ( 'NONE', #6928, #2346, #3539 ) ;
#5253 = DIRECTION ( 'NONE',  ( -0.000000000000000000, -0.000000000000000000, 1.000000000000000000 ) ) ;
#5254 = DIRECTION ( 'NONE',  ( 0.000000000000000000, 1.000000000000000000, 0.000000000000000000 ) ) ;
#5255 = PRODUCT_DEFINITION_FORMATION_WITH_SPECIFIED_SOURCE ( 'ANY', '', #7374, .NOT_KNOWN. ) ;
#5256 = PLANE ( 'NONE',  #1574 ) ;
#5257 = VERTEX_POINT ( 'NONE', #13503 ) ;
#5258 = DIRECTION ( 'NONE',  ( 0.2873478855663448850, 0.9578262852211515410, 0.000000000000000000 ) ) ;
#5259 = CARTESIAN_POINT ( 'NONE',  ( 708.1388811837590538, 164.7984674554467404, 177.5999999999999091 ) ) ;
#5260 = APPLICATION_PROTOCOL_DEFINITION ( 'draft international standard', 'automotive_design', 1998, #7062 ) ;
#5262 = VECTOR ( 'NONE', #886, 1000.000000000000000 ) ;
#5261 = LINE ( 'NONE', #13291, #3801 ) ;
#5263 = ORIENTED_EDGE ( 'NONE', *, *, #5170, .T. ) ;
#5264 = ORIENTED_EDGE ( 'NONE', *, *, #121, .T. ) ;
#5265 = CARTESIAN_POINT ( 'NONE',  ( 610.0000000000001137, 185.6790804732684705, 184.8000000000000398 ) ) ;
#5266 = DIRECTION ( 'NONE',  ( -0.000000000000000000, -0.000000000000000000, -1.000000000000000000 ) ) ;
#5267 = CARTESIAN_POINT ( 'NONE',  ( -6.500000000000000000, -3.752776749732572803, -8.000000000000000000 ) ) ;
#5268 = AXIS2_PLACEMENT_3D ( 'NONE', #3212, #11913, #1804 ) ;
#5269 = CYLINDRICAL_SURFACE ( 'NONE', #11060, 2.649999999999985700 ) ;
#5270 = ORIENTED_EDGE ( 'NONE', *, *, #8099, .T. ) ;
#5271 = DIRECTION ( 'NONE',  ( -0.9578262852211507639, 0.2873478855663477716, 0.000000000000000000 ) ) ;
#5272 = CARTESIAN_POINT ( 'NONE',  ( 610.0000000000000000, 175.0000000000000568, 210.0000000000000000 ) ) ;
#5273 = ORIENTED_EDGE ( 'NONE', *, *, #11797, .F. ) ;
#5274 = CARTESIAN_POINT ( 'NONE',  ( 703.1581845006096501, 166.2926764603917036, -149.9999999999986642 ) ) ;
#5275 = CARTESIAN_POINT ( 'NONE',  ( 6.367873360227558344, -2.886751345948134873, -5.000000000000000000 ) ) ;
#5276 = CARTESIAN_POINT ( 'NONE',  ( 635.0000000000000000, 160.0000000000000284, 211.0000000000000000 ) ) ;
#5277 = SHAPE_REPRESENTATION_RELATIONSHIP ( 'NONE' , 'NONE' ,  #6779, #7024 ) ;
#5278 = EDGE_CURVE ( 'NONE', #2790, #1880, #5002, .T. ) ;
#5279 = ORIENTED_EDGE ( 'NONE', *, *, #13115, .F. ) ;
#5280 = DIRECTION ( 'NONE',  ( 1.000000000000000000, 0.000000000000000000, 0.000000000000000000 ) ) ;
#5281 = VERTEX_POINT ( 'NONE', #8785 ) ;
#5282 = ORIENTED_EDGE ( 'NONE', *, *, #6189, .F. ) ;
#5283 = CARTESIAN_POINT ( 'NONE',  ( 0.000000000000000000, 0.000000000000000000, -0.4201245229258211977 ) ) ;
#5284 = CYLINDRICAL_SURFACE ( 'NONE', #12257, 2.649999999999985700 ) ;
#5285 = EDGE_LOOP ( 'NONE', ( #7926, #8457, #7602, #5724 ) ) ;
#5286 = VERTEX_POINT ( 'NONE', #13283 ) ;
#5287 = CARTESIAN_POINT ( 'NONE',  ( -20.63749999999999574, 0.000000000000000000, -7.500000000000000000 ) ) ;
#5288 = APPLICATION_CONTEXT ( 'automotive_design' ) ;
#5289 = DIRECTION ( 'NONE',  ( -1.000000000000000000, 0.000000000000000000, 0.000000000000000000 ) ) ;
#5290 = SHAPE_REPRESENTATION ( 'sliding channel', ( #9440 ), #13701 ) ;
#5291 = LINE ( 'NONE', #2929, #1592 ) ;
#5292 = CARTESIAN_POINT ( 'NONE',  ( 0.000000000000000000, 0.000000000000000000, 0.000000000000000000 ) ) ;
#5293 = EDGE_CURVE ( 'NONE', #4781, #3740, #3174, .T. ) ;
#5294 = ORIENTED_EDGE ( 'NONE', *, *, #5863, .T. ) ;
#5295 = FILL_AREA_STYLE_COLOUR ( '', #7053 ) ;
#5296 = CARTESIAN_POINT ( 'NONE',  ( -10.00000000000004263, 371.6790804732683569, 169.9999999999999716 ) ) ;
#5297 = VERTEX_POINT ( 'NONE', #12670 ) ;
#5298 = CARTESIAN_POINT ( 'NONE',  ( 590.0000000000000000, 0.000000000000000000, 210.0000000000000000 ) ) ;
#5299 = EDGE_CURVE ( 'NONE', #13147, #12356, #2426, .T. ) ;
#5300 = ORIENTED_EDGE ( 'NONE', *, *, #7197, .T. ) ;
#5301 = ADVANCED_FACE ( 'NONE', ( #3617 ), #4867, .F. ) ;
#5302 = CARTESIAN_POINT ( 'NONE',  ( 590.0000000000000000, 0.000000000000000000, -190.0000000000000000 ) ) ;
#5303 = DIRECTION ( 'NONE',  ( 1.000000000000000000, 0.000000000000000000, 0.000000000000000000 ) ) ;
#5304 = EDGE_CURVE ( 'NONE', #10698, #6810, #8030, .T. ) ;
#5305 = VERTEX_POINT ( 'NONE', #2564 ) ;
#5306 = DIRECTION ( 'NONE',  ( 0.000000000000000000, 0.000000000000000000, -1.000000000000000000 ) ) ;
#5307 = DIRECTION ( 'NONE',  ( -1.000000000000000000, 0.000000000000000000, 0.000000000000000000 ) ) ;
#5308 = DIRECTION ( 'NONE',  ( 0.000000000000000000, 0.000000000000000000, -1.000000000000000000 ) ) ;
#5309 = ORIENTED_EDGE ( 'NONE', *, *, #5528, .T. ) ;
#5310 = PRESENTATION_STYLE_ASSIGNMENT (( #2947 ) ) ;
#5311 = ORIENTED_EDGE ( 'NONE', *, *, #5160, .T. ) ;
#5312 = EDGE_LOOP ( 'NONE', ( #10941, #7976, #10232, #3470 ) ) ;
#5313 = DIRECTION ( 'NONE',  ( -1.000000000000000000, 0.000000000000000000, 0.000000000000000000 ) ) ;
#5314 = EDGE_CURVE ( 'NONE', #2225, #5524, #13857, .T. ) ;
#5315 = FACE_BOUND ( 'NONE', #11191, .T. ) ;
#5316 = CARTESIAN_POINT ( 'NONE',  ( 6.507056315241512401, 2.833450876375911420, -5.092319121366347900 ) ) ;
#5317 = EDGE_CURVE ( 'NONE', #8139, #3170, #11331, .T. ) ;
#5318 = DIRECTION ( 'NONE',  ( 0.9578262852211489875, -0.2873478855663534892, 0.000000000000000000 ) ) ;
#5319 = UNCERTAINTY_MEASURE_WITH_UNIT (LENGTH_MEASURE( 1.000000000000000082E-05 ), #1820, 'distance_accuracy_value', 'NONE');
#5320 = DIRECTION ( 'NONE',  ( -0.000000000000000000, -0.000000000000000000, 1.000000000000000000 ) ) ;
#5321 = ORIENTED_EDGE ( 'NONE', *, *, #3876, .T. ) ;
#5322 = CARTESIAN_POINT ( 'NONE',  ( -9.137956343300796647, 416.3137853645750397, -184.7999999999999829 ) ) ;
#5323 = CARTESIAN_POINT ( 'NONE',  ( 610.0000000000000000, -9.999999999999941380, 210.0000000000000000 ) ) ;
#5324 = DIRECTION ( 'NONE',  ( -1.000000000000000000, -0.000000000000000000, -0.000000000000000000 ) ) ;
#5325 = ORIENTED_EDGE ( 'NONE', *, *, #9990, .F. ) ;
#5326 = ORIENTED_EDGE ( 'NONE', *, *, #14113, .F. ) ;
#5327 = FACE_OUTER_BOUND ( 'NONE', #12769, .T. ) ;
#5328 = LINE ( 'NONE', #3040, #10611 ) ;
#5329 = B_SPLINE_CURVE_WITH_KNOTS ( 'NONE', 3,
 ( #6064, #360, #2604, #11386, #9250, #12481 ),
 .UNSPECIFIED., .F., .F.,
 ( 4, 2, 4 ),
 ( 0.003981881017442818506, 0.005970145066490139402, 0.007958409115537461165 ),
 .UNSPECIFIED. ) ;
#5330 = CARTESIAN_POINT ( 'NONE',  ( 609.6834941627989792, 186.8890602495695248, -187.9755619318007405 ) ) ;
#5331 = CARTESIAN_POINT ( 'NONE',  ( -6.781345014477444977, 3.590342129888853151, -6.122077150241850951 ) ) ;
#5332 = ORIENTED_EDGE ( 'NONE', *, *, #12142, .T. ) ;
#5333 = UNCERTAINTY_MEASURE_WITH_UNIT (LENGTH_MEASURE( 1.000000000000000082E-05 ), #4743, 'distance_accuracy_value', 'NONE');
#5334 = CARTESIAN_POINT ( 'NONE',  ( -6.500000000000000000, 1.392044006191029304, -6.058542048163745086 ) ) ;
#5335 = EDGE_LOOP ( 'NONE', ( #1341, #7757, #340 ) ) ;
#5336 = B_SPLINE_CURVE_WITH_KNOTS ( 'NONE', 3,
 ( #3498, #987, #3363, #1207, #9999, #2235, #5716, #8823 ),
 .UNSPECIFIED., .F., .F.,
 ( 4, 2, 2, 4 ),
 ( 2.465131517075058656E-07, 0.001183067374689851080, 0.001774477805458923299, 0.002365888236227995517 ),
 .UNSPECIFIED. ) ;
#5337 = LINE ( 'NONE', #14271, #4441 ) ;
#5338 = CARTESIAN_POINT ( 'NONE',  ( 5.200000000000002842, 0.000000000000000000, -2.700000000000000622 ) ) ;
#5339 = CARTESIAN_POINT ( 'NONE',  ( 0.000000000000000000, 0.000000000000000000, -0.2800830152838844622 ) ) ;
#5340 = VERTEX_POINT ( 'NONE', #12604 ) ;
#5341 = EDGE_CURVE ( 'NONE', #14108, #793, #3535, .T. ) ;
#5342 = CYLINDRICAL_SURFACE ( 'NONE', #12730, 0.7500000000000000000 ) ;
#5343 = ORIENTED_EDGE ( 'NONE', *, *, #13902, .T. ) ;
#5344 = ORIENTED_EDGE ( 'NONE', *, *, #9527, .F. ) ;
#5345 = CARTESIAN_POINT ( 'NONE',  ( -4.053687927322266270E-15, 4.207632145829744097, -2.712167343862821767 ) ) ;
#5346 = CARTESIAN_POINT ( 'NONE',  ( 639.0000000000000000, 156.0000000000000000, -233.5000000000000000 ) ) ;
#5347 = EDGE_CURVE ( 'NONE', #4527, #13395, #331, .T. ) ;
#5348 = ORIENTED_EDGE ( 'NONE', *, *, #3409, .F. ) ;
#5349 = EDGE_CURVE ( 'NONE', #14499, #8855, #14400, .T. ) ;
#5350 = ORIENTED_EDGE ( 'NONE', *, *, #10901, .T. ) ;
#5351 = DIRECTION ( 'NONE',  ( -1.000000000000000000, 0.000000000000000000, 0.000000000000000000 ) ) ;
#5352 = DIRECTION ( 'NONE',  ( -0.2873478855663477161, -0.9578262852211506528, 0.000000000000000000 ) ) ;
#5353 = CARTESIAN_POINT ( 'NONE',  ( -2.000000000000000000, -6.429618962271402616, -1.000000000000000000 ) ) ;
#5354 = CARTESIAN_POINT ( 'NONE',  ( -8.074769166705396017, 378.0965165842501392, -187.0000000000000284 ) ) ;
#5355 = EDGE_LOOP ( 'NONE', ( #10376, #6720 ) ) ;
#5356 = CARTESIAN_POINT ( 'NONE',  ( 609.6834941627989792, 186.8890602495695248, 187.9755619318007405 ) ) ;
#5357 = CYLINDRICAL_SURFACE ( 'NONE', #3992, 5.000000000000004441 ) ;
#5358 = ORIENTED_EDGE ( 'NONE', *, *, #11410, .T. ) ;
#5359 = DIRECTION ( 'NONE',  ( -0.9578262852211514300, 0.2873478855663454401, 0.000000000000000000 ) ) ;
#5360 = ORIENTED_EDGE ( 'NONE', *, *, #8291, .T. ) ;
#5361 = AXIS2_PLACEMENT_3D ( 'NONE', #3601, #4628, #6975 ) ;
#5362 = DIRECTION ( 'NONE',  ( -1.000000000000000000, 0.000000000000000000, 0.000000000000000000 ) ) ;
#5363 = ADVANCED_FACE ( 'NONE', ( #3756 ), #11421, .T. ) ;
#5364 = CARTESIAN_POINT ( 'NONE',  ( 0.3108895250735811411, -2.416698868092464370, 4.999999999999999112 ) ) ;
#5365 = VERTEX_POINT ( 'NONE', #5968 ) ;
#5366 = DIRECTION ( 'NONE',  ( -0.2873478855663441633, -0.9578262852211516520, 3.408579461568462910E-15 ) ) ;
#5367 = CARTESIAN_POINT ( 'NONE',  ( 650.0000000000000000, 175.0000000000000568, 210.0000000000000000 ) ) ;
#5368 = VECTOR ( 'NONE', #10515, 1000.000000000000114 ) ;
#5369 = VECTOR ( 'NONE', #12961, 1000.000000000000000 ) ;
#5370 = DIRECTION ( 'NONE',  ( -0.000000000000000000, -0.000000000000000000, -1.000000000000000000 ) ) ;
#5371 =( NAMED_UNIT ( * ) PLANE_ANGLE_UNIT ( ) SI_UNIT ( $, .RADIAN. ) );
#5372 = EDGE_LOOP ( 'NONE', ( #2331, #11282, #2467 ) ) ;
#5373 = ADVANCED_FACE ( 'NONE', ( #5810 ), #8319, .T. ) ;
#5374 = CARTESIAN_POINT ( 'NONE',  ( 703.1581845006096501, 166.2926764603917036, -177.6000000000005059 ) ) ;
#5375 = ORIENTED_EDGE ( 'NONE', *, *, #10608, .F. ) ;
#5376 = ORIENTED_EDGE ( 'NONE', *, *, #1074, .T. ) ;
#5377 = CARTESIAN_POINT ( 'NONE',  ( -0.2259792476677704443, -7.636022678937404606, -6.470294263593365791 ) ) ;
#5379 = VECTOR ( 'NONE', #1125, 1000.000000000000000 ) ;
#5378 = CARTESIAN_POINT ( 'NONE',  ( -10.00000000000000000, 0.000000000000000000, -210.0000000000000000 ) ) ;
#5380 = ADVANCED_FACE ( 'NONE', ( #8162 ), #4802, .T. ) ;
#5381 = DIRECTION ( 'NONE',  ( 0.000000000000000000, 0.000000000000000000, 1.000000000000000000 ) ) ;
#5382 = CARTESIAN_POINT ( 'NONE',  ( 639.0000000000000000, 164.0000000000000000, -225.5000000000000000 ) ) ;
#5383 = PLANE ( 'NONE',  #10053 ) ;
#5384 = EDGE_CURVE ( 'NONE', #6453, #1630, #1634, .T. ) ;
#5385 = EDGE_LOOP ( 'NONE', ( #7964, #2438 ) ) ;
#5386 = AXIS2_PLACEMENT_3D ( 'NONE', #8912, #11134, #5313 ) ;
#5387 = ADVANCED_FACE ( 'NONE', ( #10313 ), #11637, .F. ) ;
#5388 = CIRCLE ( 'NONE', #10806, 5.000000000000004441 ) ;
#5389 = AXIS2_PLACEMENT_3D ( 'NONE', #5701, #5836, #10340 ) ;
#5390 = PLANE ( 'NONE',  #8203 ) ;
#5391 = DIRECTION ( 'NONE',  ( 0.000000000000000000, 0.000000000000000000, 1.000000000000000000 ) ) ;
#5392 = PRODUCT_CONTEXT ( 'NONE', #5288, 'mechanical' ) ;
#5394 = EDGE_CURVE ( 'NONE', #9054, #11328, #13722, .T. ) ;
#5393 = DIRECTION ( 'NONE',  ( 0.000000000000000000, 0.000000000000000000, -1.000000000000000000 ) ) ;
#5395 = EDGE_LOOP ( 'NONE', ( #11149, #11866, #3007, #9629 ) ) ;
#5396 = VERTEX_POINT ( 'NONE', #6987 ) ;
#5397 = FILL_AREA_STYLE_COLOUR ( '', #3491 ) ;
#5398 = CARTESIAN_POINT ( 'NONE',  ( 642.5000000000001137, 160.0000000000000284, -225.5000000000000000 ) ) ;
#5399 = B_SPLINE_CURVE_WITH_KNOTS ( 'NONE', 3,
 ( #13556, #2189, #13490, #5582, #9121 ),
 .UNSPECIFIED., .F., .F.,
 ( 4, 1, 4 ),
 ( 0.000000000000000000, 0.002886751345948123347, 0.005773502691896246694 ),
 .UNSPECIFIED. ) ;
#5400 = CIRCLE ( 'NONE', #9163, 5.384454397937118664 ) ;
#5401 = CARTESIAN_POINT ( 'NONE',  ( 0.000000000000000000, 0.000000000000000000, -8.000000000000000000 ) ) ;
#5402 = AXIS2_PLACEMENT_3D ( 'NONE', #14562, #13379, #11169 ) ;
#5403 = VECTOR ( 'NONE', #5228, 1000.000000000000114 ) ;
#5404 = PLANE ( 'NONE',  #4990 ) ;
#5405 = VERTEX_POINT ( 'NONE', #1380 ) ;
#5406 = CARTESIAN_POINT ( 'NONE',  ( 2.999999999999999112, 0.000000000000000000, 0.000000000000000000 ) ) ;
#5407 = EDGE_LOOP ( 'NONE', ( #422, #9481, #2036, #5942 ) ) ;
#5409 = EDGE_CURVE ( 'NONE', #2660, #13868, #5885, .T. ) ;
#5408 = AXIS2_PLACEMENT_3D ( 'NONE', #2707, #3963, #4043 ) ;
#5410 = DIRECTION ( 'NONE',  ( -0.000000000000000000, -0.000000000000000000, -1.000000000000000000 ) ) ;
#5411 = LINE ( 'NONE', #8735, #13411 ) ;
#5412 = DIRECTION ( 'NONE',  ( 0.000000000000000000, 1.000000000000000000, 0.000000000000000000 ) ) ;
#5413 = SURFACE_SIDE_STYLE ('',( #5124 ) ) ;
#5414 = VERTEX_POINT ( 'NONE', #786 ) ;
#5415 = AXIS2_PLACEMENT_3D ( 'NONE', #1761, #6266, #8846 ) ;
#5416 = CARTESIAN_POINT ( 'NONE',  ( -1.400000000000000133, 0.000000000000000000, -5.100000000000000533 ) ) ;
#5417 = CONICAL_SURFACE ( 'NONE', #2586, 6.500000000000000888, 0.8987552595851582282 ) ;
#5418 = ORIENTED_EDGE ( 'NONE', *, *, #10633, .T. ) ;
#5419 = VERTEX_POINT ( 'NONE', #5150 ) ;
#5420 = CARTESIAN_POINT ( 'NONE',  ( -3.333333333333335258, 2.694301256218251783, -3.300726591567079815 ) ) ;
#5421 = DIRECTION ( 'NONE',  ( 0.000000000000000000, 0.000000000000000000, -1.000000000000000000 ) ) ;
#5422 = COLOUR_RGB ( '',0.8941176470588234615, 0.8941176470588234615, 0.8941176470588234615 ) ;
#5423 = ADVANCED_FACE ( 'NONE', ( #7434 ), #2782, .F. ) ;
#5424 = DIRECTION ( 'NONE',  ( 1.000000000000000000, 0.000000000000000000, 0.000000000000000000 ) ) ;
#5425 = VECTOR ( 'NONE', #3533, 1000.000000000000000 ) ;
#5426 = EDGE_CURVE ( 'NONE', #264, #734, #14017, .T. ) ;
#5427 = ORIENTED_EDGE ( 'NONE', *, *, #3435, .T. ) ;
#5428 = ORIENTED_EDGE ( 'NONE', *, *, #9139, .T. ) ;
#5429 = FACE_BOUND ( 'NONE', #7934, .T. ) ;
#5430 = CARTESIAN_POINT ( 'NONE',  ( 639.0000000000000000, 164.0000000000000000, -233.5000000000000000 ) ) ;
#5431 = DIRECTION ( 'NONE',  ( 1.000000000000000000, 0.000000000000000000, 0.000000000000000000 ) ) ;
#5432 = LINE ( 'NONE', #6396, #6551 ) ;
#5433 = PLANE ( 'NONE',  #4092 ) ;
#5434 = AXIS2_PLACEMENT_3D ( 'NONE', #13521, #9151, #2442 ) ;
#5435 = ORIENTED_EDGE ( 'NONE', *, *, #14466, .F. ) ;
#5436 = AXIS2_PLACEMENT_3D ( 'NONE', #2176, #10149, #236 ) ;
#5437 = CARTESIAN_POINT ( 'NONE',  ( 8.500000000000000000, 2.886751345948122882, -5.000000000000000000 ) ) ;
#5438 = EDGE_LOOP ( 'NONE', ( #11345, #1067 ) ) ;
#5439 = DIRECTION ( 'NONE',  ( 0.000000000000000000, 0.000000000000000000, 1.000000000000000000 ) ) ;
#5440 = CIRCLE ( 'NONE', #3554, 5.000000000000004441 ) ;
#5441 = ORIENTED_EDGE ( 'NONE', *, *, #11512, .T. ) ;
#5442 = CYLINDRICAL_SURFACE ( 'NONE', #12489, 5.199999999999999289 ) ;
#5443 = VECTOR ( 'NONE', #6497, 1000.000000000000000 ) ;
#5444 = VECTOR ( 'NONE', #2450, 1000.000000000000114 ) ;
#5445 = DIRECTION ( 'NONE',  ( -1.000000000000000000, 0.000000000000000000, 0.000000000000000000 ) ) ;
#5446 = ORIENTED_EDGE ( 'NONE', *, *, #13336, .T. ) ;
#5447 = CARTESIAN_POINT ( 'NONE',  ( 2.855764796983346177, -2.970025579236428737, -0.09382832055446485575 ) ) ;
#5448 = CARTESIAN_POINT ( 'NONE',  ( -12.99999999999999112, -3.903127820947815962E-15, 0.000000000000000000 ) ) ;
#5449 = AXIS2_PLACEMENT_3D ( 'NONE', #4724, #10529, #9215 ) ;
#5450 =( GEOMETRIC_REPRESENTATION_CONTEXT ( 3 ) GLOBAL_UNCERTAINTY_ASSIGNED_CONTEXT ( ( #2807 ) ) GLOBAL_UNIT_ASSIGNED_CONTEXT ( ( #555, #1672, #6246 ) ) REPRESENTATION_CONTEXT ( 'NONE', 'WORKASPACE' ) );
#5451 = DIRECTION ( 'NONE',  ( 0.000000000000000000, -1.000000000000000000, 1.287488025362403787E-15 ) ) ;
#5452 =( NAMED_UNIT ( * ) SI_UNIT ( $, .STERADIAN. ) SOLID_ANGLE_UNIT ( ) );
#5453 = EDGE_LOOP ( 'NONE', ( #3243, #5815, #2472, #1556 ) ) ;
#5454 = ORIENTED_EDGE ( 'NONE', *, *, #5481, .F. ) ;
#5455 = CIRCLE ( 'NONE', #960, 7.000000000000000000 ) ;
#5456 = EDGE_CURVE ( 'NONE', #10831, #10448, #8685, .T. ) ;
#5457 = AXIS2_PLACEMENT_3D ( 'NONE', #7158, #6937, #11713 ) ;
#5458 = VERTEX_POINT ( 'NONE', #7282 ) ;
#5459 = DIRECTION ( 'NONE',  ( 0.000000000000000000, 0.000000000000000000, -1.000000000000000000 ) ) ;
#5460 = AXIS2_PLACEMENT_3D ( 'NONE', #10689, #14160, #564 ) ;
#5461 =( GEOMETRIC_REPRESENTATION_CONTEXT ( 3 ) GLOBAL_UNCERTAINTY_ASSIGNED_CONTEXT ( ( #6051 ) ) GLOBAL_UNIT_ASSIGNED_CONTEXT ( ( #12580, #5640, #6898 ) ) REPRESENTATION_CONTEXT ( 'NONE', 'WORKASPACE' ) );
#5462 = SHAPE_REPRESENTATION ( 'hex bolt gradeab_iso_ISO 4014 - M5 x 30 x 16-N', ( #9440 ), #5943 ) ;
#5463 = CARTESIAN_POINT ( 'NONE',  ( 640.0000000000000000, 160.0000000000000284, -187.5000000000000000 ) ) ;
#5464 = CARTESIAN_POINT ( 'NONE',  ( 635.9940618270015875, 167.4999005938269079, -210.0000000000000000 ) ) ;
#5465 = AXIS2_PLACEMENT_3D ( 'NONE', #7927, #11319, #12416 ) ;
#5466 = DIRECTION ( 'NONE',  ( 0.3543563944859323689, -0.9351104457158684324, 0.000000000000000000 ) ) ;
#5467 = CARTESIAN_POINT ( 'NONE',  ( 4.000000000000000000, 0.000000000000000000, 0.000000000000000000 ) ) ;
#5468 = LINE ( 'NONE', #4361, #10058 ) ;
#5469 = ORIENTED_EDGE ( 'NONE', *, *, #5034, .F. ) ;
#5470 = DIRECTION ( 'NONE',  ( -0.9578262852211514300, 0.2873478855663454956, -1.399211572952243085E-16 ) ) ;
#5471 = CARTESIAN_POINT ( 'NONE',  ( 228.5935732249375008, 306.3651924111313178, -177.6000000000005059 ) ) ;
#5472 = SHAPE_DEFINITION_REPRESENTATION ( #4395, #748 ) ;
#5473 = ADVANCED_FACE ( 'NONE', ( #8613 ), #8545, .T. ) ;
#5474 = CARTESIAN_POINT ( 'NONE',  ( 42.80949999999999278, 0.000000000000000000, 0.000000000000000000 ) ) ;
#5475 = EDGE_LOOP ( 'NONE', ( #4124, #6166, #3690, #2497 ) ) ;
#5476 = EDGE_LOOP ( 'NONE', ( #4268, #7297, #14511, #5723 ) ) ;
#5477 = AXIS2_PLACEMENT_3D ( 'NONE', #8035, #12608, #12537 ) ;
#5478 = CARTESIAN_POINT ( 'NONE',  ( -2.688821387764050996E-14, -4.618802153517012954, -0.4999999999999995559 ) ) ;
#5479 = ADVANCED_FACE ( 'NONE', ( #12897 ), #10874, .T. ) ;
#5480 = FACE_OUTER_BOUND ( 'NONE', #3413, .T. ) ;
#5481 = EDGE_CURVE ( 'NONE', #6009, #2433, #10613, .T. ) ;
#5482 = CARTESIAN_POINT ( 'NONE',  ( 639.0000000000000000, 164.0000000000000000, -233.5000000000000000 ) ) ;
#5483 = ORIENTED_EDGE ( 'NONE', *, *, #3310, .T. ) ;
#5484 = EDGE_CURVE ( 'NONE', #13279, #5305, #964, .T. ) ;
#5485 = CIRCLE ( 'NONE', #995, 4.199999999999981526 ) ;
#5486 = CARTESIAN_POINT ( 'NONE',  ( 611.4942090049448780, 232.4210031920598283, 184.7999999999999829 ) ) ;
#5487 = VERTEX_POINT ( 'NONE', #3906 ) ;
#5488 = DIRECTION ( 'NONE',  ( -1.000000000000000000, 0.000000000000000000, 0.000000000000000000 ) ) ;
#5489 = DIRECTION ( 'NONE',  ( 0.000000000000000000, 0.000000000000000000, -1.000000000000000000 ) ) ;
#5490 = CARTESIAN_POINT ( 'NONE',  ( 610.0000000000002274, 185.6790804732683284, -169.9999999999999716 ) ) ;
#5491 = CARTESIAN_POINT ( 'NONE',  ( 610.0000000000001137, 191.1080398579018720, -187.0000000000000000 ) ) ;
#5492 = ORIENTED_EDGE ( 'NONE', *, *, #13336, .F. ) ;
#5493 = VERTEX_POINT ( 'NONE', #8388 ) ;
#5494 = B_SPLINE_CURVE_WITH_KNOTS ( 'NONE', 3,
 ( #348, #13961, #4747, #4884, #5908, #1330, #3555, #9378, #9152, #8051, #3636, #428, #6870, #8261, #12772, #122 ),
 .UNSPECIFIED., .F., .F.,
 ( 4, 3, 3, 3, 3, 4 ),
 ( 0.000000000000000000, 5.303647860849928001E-05, 0.0001057093501027655180, 0.0001642058037234009067, 0.0002210073443967662933, 0.0002236769549551740374 ),
 .UNSPECIFIED. ) ;
#5495 = CARTESIAN_POINT ( 'NONE',  ( 0.08165819712376794215, 3.720292241887086071, -3.556264818047238041 ) ) ;
#5496 = DIRECTION ( 'NONE',  ( -1.000000000000000000, 0.000000000000000000, 0.000000000000000000 ) ) ;
#5497 = CIRCLE ( 'NONE', #5041, 2.199999999999693312 ) ;
#5498 = EDGE_CURVE ( 'NONE', #5961, #14241, #10830, .T. ) ;
#5499 = EDGE_CURVE ( 'NONE', #3047, #7440, #12039, .T. ) ;
#5500 = LINE ( 'NONE', #4455, #10384 ) ;
#5501 = ORIENTED_EDGE ( 'NONE', *, *, #12145, .T. ) ;
#5502 = ADVANCED_FACE ( 'NONE', ( #9515 ), #9733, .F. ) ;
#5503 = ORIENTED_EDGE ( 'NONE', *, *, #5742, .T. ) ;
#5504 = CARTESIAN_POINT ( 'NONE',  ( 609.6990281814310038, 187.8427340524074225, -188.9822575857425022 ) ) ;
#5505 = CARTESIAN_POINT ( 'NONE',  ( 629.7500000000000000, 160.0000000000000284, -210.0000000000000000 ) ) ;
#5506 = CARTESIAN_POINT ( 'NONE',  ( 124.4591373975826514, 414.8637913252776457, 0.000000000000000000 ) ) ;
#5507 = DIRECTION ( 'NONE',  ( 0.000000000000000000, -0.000000000000000000, 1.000000000000000000 ) ) ;
#5508 = CARTESIAN_POINT ( 'NONE',  ( 0.1920286436967153787, 0.000000000000000000, 5.525000000000000355 ) ) ;
#5509 =( NAMED_UNIT ( * ) SI_UNIT ( $, .STERADIAN. ) SOLID_ANGLE_UNIT ( ) );
#5510 = ORIENTED_EDGE ( 'NONE', *, *, #141, .F. ) ;
#5511 =( NAMED_UNIT ( * ) PLANE_ANGLE_UNIT ( ) SI_UNIT ( $, .RADIAN. ) );
#5512 = CONTEXT_DEPENDENT_SHAPE_REPRESENTATION ( #162, #12565 ) ;
#5513 = ORIENTED_EDGE ( 'NONE', *, *, #9087, .F. ) ;
#5514 = PLANE ( 'NONE',  #13461 ) ;
#5515 = ORIENTED_EDGE ( 'NONE', *, *, #392, .T. ) ;
#5516 = FACE_OUTER_BOUND ( 'NONE', #5014, .T. ) ;
#5517 = CARTESIAN_POINT ( 'NONE',  ( 635.0000000000000000, 160.0000000000000284, -210.0000119999999981 ) ) ;
#5518 = VERTEX_POINT ( 'NONE', #9581 ) ;
#5519 = DIRECTION ( 'NONE',  ( 1.000000000000000000, 0.000000000000000000, -0.000000000000000000 ) ) ;
#5520 = DIRECTION ( 'NONE',  ( -1.000000000000000000, -0.000000000000000000, -0.000000000000000000 ) ) ;
#5521 = DIRECTION ( 'NONE',  ( 0.9578262852211507639, -0.2873478855663477716, -0.000000000000000000 ) ) ;
#5522 = ORIENTED_EDGE ( 'NONE', *, *, #8833, .F. ) ;
#5523 = ORIENTED_EDGE ( 'NONE', *, *, #12173, .T. ) ;
#5524 = VERTEX_POINT ( 'NONE', #3971 ) ;
#5525 = CARTESIAN_POINT ( 'NONE',  ( -3.755786496842903988E-16, -7.505553499465146494, -8.000000000000000000 ) ) ;
#5526 = PLANE ( 'NONE',  #10125 ) ;
#5527 = CARTESIAN_POINT ( 'NONE',  ( 2.805705207896068476, -3.226868319750173075, -3.503898532754370354 ) ) ;
#5528 = EDGE_CURVE ( 'NONE', #3014, #2441, #13709, .T. ) ;
#5529 = CARTESIAN_POINT ( 'NONE',  ( -4.000000000000000000, -2.309401076758512694, -3.433295621305382461 ) ) ;
#5530 = ADVANCED_FACE ( 'NONE', ( #14235, #9796 ), #12973, .F. ) ;
#5531 = FACE_OUTER_BOUND ( 'NONE', #10622, .T. ) ;
#5532 = CARTESIAN_POINT ( 'NONE',  ( 0.3572655899081558228, -2.309401076758485161, 3.999999999999999112 ) ) ;
#5533 = DIRECTION ( 'NONE',  ( -0.2873478855663454401, -0.9578262852211514300, -4.197634718856730240E-17 ) ) ;
#5534 = ORIENTED_EDGE ( 'NONE', *, *, #13630, .F. ) ;
#5535 = CARTESIAN_POINT ( 'NONE',  ( -9.137956343300944084, 416.3137853645740734, 190.0000000000000000 ) ) ;
#5536 = DIRECTION ( 'NONE',  ( 0.9995235871707960351, -0.03086419753086420970, 0.000000000000000000 ) ) ;
#5537 = SHAPE_DEFINITION_REPRESENTATION ( #2890, #14430 ) ;
#5538 = CARTESIAN_POINT ( 'NONE',  ( -6.500000000000000000, 3.752776749732564809, -6.064240316920399110 ) ) ;
#5539 = VERTEX_POINT ( 'NONE', #1750 ) ;
#5540 = ORIENTED_EDGE ( 'NONE', *, *, #9620, .F. ) ;
#5541 =( NAMED_UNIT ( * ) PLANE_ANGLE_UNIT ( ) SI_UNIT ( $, .RADIAN. ) );
#5542 = DIRECTION ( 'NONE',  ( -0.9578262852211514300, 0.2873478855663454401, 0.000000000000000000 ) ) ;
#5543 = CARTESIAN_POINT ( 'NONE',  ( 0.000000000000000000, 0.000000000000000000, -7.554475477074173106 ) ) ;
#5544 = EDGE_CURVE ( 'NONE', #13410, #12823, #10751, .T. ) ;
#5545 = CARTESIAN_POINT ( 'NONE',  ( -9.137956343300944084, 416.3137853645740734, 190.0000000000000000 ) ) ;
#5546 = ORIENTED_EDGE ( 'NONE', *, *, #7454, .T. ) ;
#5547 = CARTESIAN_POINT ( 'NONE',  ( 6.323279575528021113, -5.335162385627945980, -0.7592276814620767533 ) ) ;
#5548 = VERTEX_POINT ( 'NONE', #4053 ) ;
#5549 = FACE_OUTER_BOUND ( 'NONE', #2501, .T. ) ;
#5550 = CARTESIAN_POINT ( 'NONE',  ( -8.074769166705396017, 378.0965165842501392, 187.0000000000000284 ) ) ;
#5551 = VECTOR ( 'NONE', #1407, 1000.000000000000000 ) ;
#5552 = EDGE_CURVE ( 'NONE', #1836, #5769, #7502, .T. ) ;
#5553 = DIRECTION ( 'NONE',  ( 0.000000000000000000, -0.000000000000000000, 1.000000000000000000 ) ) ;
#5554 = VERTEX_POINT ( 'NONE', #10910 ) ;
#5555 = ORIENTED_EDGE ( 'NONE', *, *, #6621, .T. ) ;
#5556 = DIRECTION ( 'NONE',  ( -0.000000000000000000, -0.000000000000000000, -1.000000000000000000 ) ) ;
#5557 = DIRECTION ( 'NONE',  ( 1.000000000000000000, 0.000000000000000000, 0.000000000000000000 ) ) ;
#5558 = CARTESIAN_POINT ( 'NONE',  ( 152.8304684875957662, 364.5911659626319761, 210.0000000000000000 ) ) ;
#5559 = ADVANCED_FACE ( 'NONE', ( #4187 ), #8045, .F. ) ;
#5560 = ORIENTED_EDGE ( 'NONE', *, *, #10251, .T. ) ;
#5561 = ORIENTED_EDGE ( 'NONE', *, *, #8621, .F. ) ;
#5562 = CARTESIAN_POINT ( 'NONE',  ( 609.6829874266189790, 186.4320250235422805, -187.4339272673398398 ) ) ;
#5563 = CARTESIAN_POINT ( 'NONE',  ( -1.399999999999999689, 9.062386313690412402E-16, 7.399999999999999467 ) ) ;
#5564 = CARTESIAN_POINT ( 'NONE',  ( -2.807080416178626692, 3.225969019225154444, -3.502507215260441065 ) ) ;
#5565 = CARTESIAN_POINT ( 'NONE',  ( -0.6507732100473471171, 4.243078065514775510, -0.2236248678334823436 ) ) ;
#5566 = CYLINDRICAL_SURFACE ( 'NONE', #7145, 4.199999999999926459 ) ;
#5567 = PRODUCT ( 'hex flange nut gradea_iso_ISO - 4161 - M8 - N', 'hex flange nut gradea_iso_ISO - 4161 - M8 - N', '', ( #655 ) ) ;
#5568 = EDGE_LOOP ( 'NONE', ( #2377, #9073 ) ) ;
#5569 = EDGE_CURVE ( 'NONE', #8728, #11174, #2866, .T. ) ;
#5570 = CARTESIAN_POINT ( 'NONE',  ( 164.3243839102495656, 402.9042173714779551, 190.0000000000000000 ) ) ;
#5571 = VERTEX_POINT ( 'NONE', #7587 ) ;
#5572 = ORIENTED_EDGE ( 'NONE', *, *, #4113, .F. ) ;
#5573 = FACE_OUTER_BOUND ( 'NONE', #2944, .T. ) ;
#5574 = ADVANCED_FACE ( 'NONE', ( #11122 ), #1003, .F. ) ;
#5575 = ORIENTED_EDGE ( 'NONE', *, *, #1146, .T. ) ;
#5576 = CARTESIAN_POINT ( 'NONE',  ( 640.0000000000000000, 160.0000000000000284, 215.5000000000000000 ) ) ;
#5577 = FACE_OUTER_BOUND ( 'NONE', #1217, .T. ) ;
#5578 = VECTOR ( 'NONE', #5682, 1000.000000000000000 ) ;
#5579 = ORIENTED_EDGE ( 'NONE', *, *, #5949, .F. ) ;
#5580 = DIRECTION ( 'NONE',  ( 1.000000000000000000, 0.000000000000000000, 0.000000000000000000 ) ) ;
#5581 = FACE_OUTER_BOUND ( 'NONE', #3646, .T. ) ;
#5582 = CARTESIAN_POINT ( 'NONE',  ( 6.196878017913834746, 1.924500897298752289, 5.000000000000000000 ) ) ;
#5583 = DIRECTION ( 'NONE',  ( 1.000000000000000000, 0.000000000000000000, 0.000000000000000000 ) ) ;
#5584 = ORIENTED_EDGE ( 'NONE', *, *, #3407, .F. ) ;
#5585 = LINE ( 'NONE', #4796, #12004 ) ;
#5586 = AXIS2_PLACEMENT_3D ( 'NONE', #1580, #9497, #7267 ) ;
#5587 = EDGE_LOOP ( 'NONE', ( #8626, #7292 ) ) ;
#5588 = PRODUCT_DEFINITION ( 'UNKNOWN', '', #13981, #6159 ) ;
#5589 = ORIENTED_EDGE ( 'NONE', *, *, #8262, .T. ) ;
#5590 = CARTESIAN_POINT ( 'NONE',  ( 635.0000000000000000, 160.0000000000000284, -210.0000000000000000 ) ) ;
#5591 = CARTESIAN_POINT ( 'NONE',  ( 107.2182642636026202, 357.3942142120087055, -210.0000000000000000 ) ) ;
#5592 = LINE ( 'NONE', #41, #7566 ) ;
#5593 = AXIS2_PLACEMENT_3D ( 'NONE', #3463, #5817, #13573 ) ;
#5594 = EDGE_CURVE ( 'NONE', #12155, #4614, #14585, .T. ) ;
#5595 = AXIS2_PLACEMENT_3D ( 'NONE', #3587, #13608, #2463 ) ;
#5596 = CARTESIAN_POINT ( 'NONE',  ( 590.0000000000000000, 212.5596934910894333, -210.0000000000000000 ) ) ;
#5597 = EDGE_CURVE ( 'NONE', #10404, #4280, #6696, .T. ) ;
#5598 = CIRCLE ( 'NONE', #9379, 5.000000000000000000 ) ;
#5599 = CARTESIAN_POINT ( 'NONE',  ( 3.250000000000004441, 5.629165124598849879, 0.000000000000000000 ) ) ;
#5600 = CARTESIAN_POINT ( 'NONE',  ( 8.331345277524542681, 0.000000000000000000, -8.000000000000000000 ) ) ;
#5601 = CARTESIAN_POINT ( 'NONE',  ( 3.678949249685231848, 0.000000000000000000, 0.000000000000000000 ) ) ;
#5602 = ORIENTED_EDGE ( 'NONE', *, *, #7666, .T. ) ;
#5603 = B_SPLINE_CURVE_WITH_KNOTS ( 'NONE', 3,
 ( #6957, #9253, #7247, #2741, #13982, #9394, #13821, #2455 ),
 .UNSPECIFIED., .F., .F.,
 ( 4, 2, 2, 4 ),
 ( 2.459764730722484167E-07, 0.001920659145285713056, 0.002880865729692032307, 0.003841072314098351557 ),
 .UNSPECIFIED. ) ;
#5604 = CARTESIAN_POINT ( 'NONE',  ( 6.436591462021368670, -5.789018756751906025, 5.182398524903814613E-16 ) ) ;
#5605 = SHAPE_DEFINITION_REPRESENTATION ( #3452, #3781 ) ;
#5606 = FACE_OUTER_BOUND ( 'NONE', #11671, .T. ) ;
#5607 = AXIS2_PLACEMENT_3D ( 'NONE', #8210, #11611, #10 ) ;
#5608 = ORIENTED_EDGE ( 'NONE', *, *, #5783, .F. ) ;
#5609 = ORIENTED_EDGE ( 'NONE', *, *, #9595, .T. ) ;
#5610 = SURFACE_STYLE_FILL_AREA ( #7688 ) ;
#5611 = DIRECTION ( 'NONE',  ( 1.000000000000000000, 0.000000000000000000, 0.000000000000000000 ) ) ;
#5612 = EDGE_CURVE ( 'NONE', #6145, #13614, #6755, .T. ) ;
#5613 = CARTESIAN_POINT ( 'NONE',  ( 10.00000000000000000, 10.00000000000000178, -210.0000000000000000 ) ) ;
#5614 = DIRECTION ( 'NONE',  ( -1.000000000000000000, 0.000000000000000000, 0.000000000000000000 ) ) ;
#5616 = ORIENTED_EDGE ( 'NONE', *, *, #13041, .F. ) ;
#5615 = VECTOR ( 'NONE', #4800, 1000.000000000000000 ) ;
#5617 = AXIS2_PLACEMENT_3D ( 'NONE', #12629, #2510, #7016 ) ;
#5618 = VECTOR ( 'NONE', #4376, 1000.000000000000114 ) ;
#5619 = CARTESIAN_POINT ( 'NONE',  ( 6.245824673232850621, -3.903127342723632154, -3.450227696316233494 ) ) ;
#5620 = ORIENTED_EDGE ( 'NONE', *, *, #7667, .T. ) ;
#5621 = PLANE ( 'NONE',  #11704 ) ;
#5622 = DIRECTION ( 'NONE',  ( 0.000000000000000000, 0.000000000000000000, -1.000000000000000000 ) ) ;
#5623 = DIRECTION ( 'NONE',  ( -1.000000000000000000, 0.000000000000000000, 0.000000000000000000 ) ) ;
#5624 = EDGE_LOOP ( 'NONE', ( #4777, #1328, #3425, #14458 ) ) ;
#5625 = ORIENTED_EDGE ( 'NONE', *, *, #2363, .T. ) ;
#5626 = DIRECTION ( 'NONE',  ( 0.000000000000000000, 0.000000000000000000, 1.000000000000000000 ) ) ;
#5627 = EDGE_CURVE ( 'NONE', #1238, #6877, #1200, .T. ) ;
#5628 = AXIS2_PLACEMENT_3D ( 'NONE', #7280, #11635, #11856 ) ;
#5629 = AXIS2_PLACEMENT_3D ( 'NONE', #1170, #13431, #1092 ) ;
#5630 = CARTESIAN_POINT ( 'NONE',  ( -9.137956343301000928, 374.5525593289319204, -169.9999999999999716 ) ) ;
#5631 = CARTESIAN_POINT ( 'NONE',  ( 4.000000000000000000, 1.680228229147133767, -3.316631783032546021 ) ) ;
#5632 = PRESENTATION_LAYER_ASSIGNMENT (  '', '', ( #11995 ) ) ;
#5633 = ORIENTED_EDGE ( 'NONE', *, *, #3511, .F. ) ;
#5634 = VERTEX_POINT ( 'NONE', #4341 ) ;
#5635 = CARTESIAN_POINT ( 'NONE',  ( 609.7043258424479291, 187.8603929224640581, -188.9582675804705332 ) ) ;
#5636 = CARTESIAN_POINT ( 'NONE',  ( 144.7991633467111683, 386.6211705227183870, 210.0000000000000000 ) ) ;
#5637 = VECTOR ( 'NONE', #4370, 1000.000000000000000 ) ;
#5638 = PLANE ( 'NONE',  #1599 ) ;
#5639 = CARTESIAN_POINT ( 'NONE',  ( 451.6722694765949768, 316.6998517015743460, -190.0000000000000000 ) ) ;
#5640 =( NAMED_UNIT ( * ) PLANE_ANGLE_UNIT ( ) SI_UNIT ( $, .RADIAN. ) );
#5641 = EDGE_LOOP ( 'NONE', ( #6120, #797, #86, #11288 ) ) ;
#5642 = CARTESIAN_POINT ( 'NONE',  ( 707.0389973793289755, 162.8315651648157427, 177.6000000000001648 ) ) ;
#5643 = ORIENTED_EDGE ( 'NONE', *, *, #677, .T. ) ;
#5644 = EDGE_LOOP ( 'NONE', ( #14425, #2919, #13157, #3207 ) ) ;
#5645 = DIRECTION ( 'NONE',  ( -1.000000000000000000, 0.000000000000000000, 0.000000000000000000 ) ) ;
#5646 = EDGE_CURVE ( 'NONE', #10297, #13338, #10454, .T. ) ;
#5647 = AXIS2_PLACEMENT_3D ( 'NONE', #323, #700, #14228 ) ;
#5648 = EDGE_LOOP ( 'NONE', ( #9234, #639, #7110, #3266, #11379 ) ) ;
#5649 = ADVANCED_FACE ( 'NONE', ( #5577 ), #9864, .F. ) ;
#5650 = CIRCLE ( 'NONE', #2585, 5.199999999999760369 ) ;
#5651 = VECTOR ( 'NONE', #3894, 1000.000000000000000 ) ;
#5652 = DIRECTION ( 'NONE',  ( -0.5000000000000051070, 0.000000000000000000, 0.8660254037844355990 ) ) ;
#5653 = AXIS2_PLACEMENT_3D ( 'NONE', #5090, #8169, #11642 ) ;
#5654 = CARTESIAN_POINT ( 'NONE',  ( 470.8287951810180516, 310.9528939902474463, 210.0000000000000000 ) ) ;
#5655 = EDGE_CURVE ( 'NONE', #8377, #1538, #4267, .T. ) ;
#5656 = VECTOR ( 'NONE', #10953, 1000.000000000000000 ) ;
#5657 = ORIENTED_EDGE ( 'NONE', *, *, #9348, .T. ) ;
#5658 = DIRECTION ( 'NONE',  ( -0.8191520442889923537, 1.003171929053525363E-16, 0.5735764363510453823 ) ) ;
#5659 = LINE ( 'NONE', #1073, #7526 ) ;
#5660 = CIRCLE ( 'NONE', #10848, 7.000000000000006217 ) ;
#5661 = EDGE_CURVE ( 'NONE', #3159, #1078, #12146, .T. ) ;
#5662 = CARTESIAN_POINT ( 'NONE',  ( -4.197393957002303999, -7.773935952363655451E-14, -3.503767560748929810 ) ) ;
#5663 = EDGE_LOOP ( 'NONE', ( #6542, #10368, #11385, #5643 ) ) ;
#5664 = VECTOR ( 'NONE', #5424, 1000.000000000000000 ) ;
#5665 = VECTOR ( 'NONE', #11280, 1000.000000000000114 ) ;
#5666 = DIRECTION ( 'NONE',  ( 1.000000000000000000, 0.000000000000000000, 0.000000000000000000 ) ) ;
#5667 = VERTEX_POINT ( 'NONE', #6545 ) ;
#5668 = ORIENTED_EDGE ( 'NONE', *, *, #9890, .T. ) ;
#5670 = CARTESIAN_POINT ( 'NONE',  ( 6.878751942472530523, -3.924677726130933575, -6.573129608219091757 ) ) ;
#5669 = CIRCLE ( 'NONE', #13927, 5.249999999999976907 ) ;
#5671 = AXIS2_PLACEMENT_3D ( 'NONE', #7966, #6653, #1175 ) ;
#5672 = DIRECTION ( 'NONE',  ( 0.000000000000000000, 0.000000000000000000, -1.000000000000000000 ) ) ;
#5673 = EDGE_CURVE ( 'NONE', #6493, #739, #2184, .T. ) ;
#5675 = CARTESIAN_POINT ( 'NONE',  ( 628.4515058436089703, 163.7887212390026832, -210.0000000000000284 ) ) ;
#5674 = AXIS2_PLACEMENT_3D ( 'NONE', #12228, #5381, #7951 ) ;
#5676 = ADVANCED_FACE ( 'NONE', ( #13485 ), #3379, .F. ) ;
#5677 = PLANE ( 'NONE',  #2862 ) ;
#5678 = ADVANCED_FACE ( 'NONE', ( #14452 ), #3221, .T. ) ;
#5679 = CARTESIAN_POINT ( 'NONE',  ( 0.1586754815284836251, -4.240386000424027024, -0.6554360035617921021 ) ) ;
#5680 = FACE_OUTER_BOUND ( 'NONE', #14377, .T. ) ;
#5681 = VECTOR ( 'NONE', #11510, 1000.000000000000114 ) ;
#5682 = DIRECTION ( 'NONE',  ( 0.9578262852211514300, -0.2873478855663452736, 1.110223024625156540E-15 ) ) ;
#5683 = EDGE_LOOP ( 'NONE', ( #11116, #118 ) ) ;
#5684 = CIRCLE ( 'NONE', #6164, 2.500000000000000444 ) ;
#5685 = CARTESIAN_POINT ( 'NONE',  ( -2.055025722541619970, -6.319083845364135144, -5.720331885005373707 ) ) ;
#5686 = DIRECTION ( 'NONE',  ( -0.2873478855663453846, -0.9578262852211513190, -0.000000000000000000 ) ) ;
#5687 = SHAPE_DEFINITION_REPRESENTATION ( #6309, #9980 ) ;
#5688 = VERTEX_POINT ( 'NONE', #12206 ) ;
#5689 = AXIS2_PLACEMENT_3D ( 'NONE', #21, #10078, #4562 ) ;
#5690 = DIRECTION ( 'NONE',  ( 0.9578262852211514300, -0.2873478855663454401, 0.000000000000000000 ) ) ;
#5691 = ORIENTED_EDGE ( 'NONE', *, *, #10068, .F. ) ;
#5692 = VERTEX_POINT ( 'NONE', #8836 ) ;
#5693 = DIRECTION ( 'NONE',  ( 1.000000000000000000, 0.000000000000000000, 0.000000000000000000 ) ) ;
#5694 = CARTESIAN_POINT ( 'NONE',  ( 6.196878017913830305, 5.292377467571570016, -0.8333333333333337034 ) ) ;
#5695 = DIRECTION ( 'NONE',  ( -0.000000000000000000, -0.000000000000000000, -1.000000000000000000 ) ) ;
#5696 = CIRCLE ( 'NONE', #2387, 2.649999999999985700 ) ;
#5697 = VECTOR ( 'NONE', #5947, 1000.000000000000000 ) ;
#5698 = FACE_OUTER_BOUND ( 'NONE', #11324, .T. ) ;
#5699 = DIRECTION ( 'NONE',  ( 0.000000000000000000, 1.000000000000000000, 0.000000000000000000 ) ) ;
#5700 = ORIENTED_EDGE ( 'NONE', *, *, #123, .F. ) ;
#5701 = CARTESIAN_POINT ( 'NONE',  ( -6.259644161404860030E-16, -4.618802153517027165, -5.000000000000000000 ) ) ;
#5702 = DIRECTION ( 'NONE',  ( 1.000000000000000000, 0.000000000000000000, 0.000000000000000000 ) ) ;
#5703 = AXIS2_PLACEMENT_3D ( 'NONE', #11104, #4688, #8960 ) ;
#5704 = LINE ( 'NONE', #3265, #14386 ) ;
#5705 = ORIENTED_EDGE ( 'NONE', *, *, #9090, .F. ) ;
#5706 = EDGE_LOOP ( 'NONE', ( #2192, #8047, #9060, #11679 ) ) ;
#5707 = DIRECTION ( 'NONE',  ( -1.000000000000000000, 0.000000000000000000, 0.000000000000000000 ) ) ;
#5708 = MECHANICAL_DESIGN_GEOMETRIC_PRESENTATION_REPRESENTATION (  '', ( #8771 ), #10652 ) ;
#5709 = DIRECTION ( 'NONE',  ( -1.000000000000000000, -0.000000000000000000, -0.000000000000000000 ) ) ;
#5710 = FACE_OUTER_BOUND ( 'NONE', #10408, .T. ) ;
#5711 = CONICAL_SURFACE ( 'NONE', #9495, 4.000000000000000000, 1.047197551196600296 ) ;
#5712 = EDGE_LOOP ( 'NONE', ( #11916, #7838, #2879, #6900 ) ) ;
#5713 = ORIENTED_EDGE ( 'NONE', *, *, #4212, .T. ) ;
#5714 = DIRECTION ( 'NONE',  ( -1.000000000000000000, 0.000000000000000000, 0.000000000000000000 ) ) ;
#5715 = ADVANCED_FACE ( 'NONE', ( #13331 ), #2102, .T. ) ;
#5716 = CARTESIAN_POINT ( 'NONE',  ( 1.828356344711641102, 3.563200125723180900, -5.433716356636336675E-16 ) ) ;
#5717 = AXIS2_PLACEMENT_3D ( 'NONE', #11518, #6056, #6950 ) ;
#5718 = DIRECTION ( 'NONE',  ( -0.000000000000000000, -0.000000000000000000, -1.000000000000000000 ) ) ;
#5719 = LINE ( 'NONE', #7996, #3966 ) ;
#5720 = FACE_OUTER_BOUND ( 'NONE', #9989, .T. ) ;
#5721 = VERTEX_POINT ( 'NONE', #5654 ) ;
#5722 = DIRECTION ( 'NONE',  ( -1.000000000000000000, -0.000000000000000000, -0.000000000000000000 ) ) ;
#5723 = ORIENTED_EDGE ( 'NONE', *, *, #2612, .T. ) ;
#5724 = ORIENTED_EDGE ( 'NONE', *, *, #918, .T. ) ;
#5725 = DIRECTION ( 'NONE',  ( 0.000000000000000000, -0.000000000000000000, 1.000000000000000000 ) ) ;
#5726 = AXIS2_PLACEMENT_3D ( 'NONE', #6000, #12937, #2745 ) ;
#5727 = ORIENTED_EDGE ( 'NONE', *, *, #7269, .T. ) ;
#5728 = DIRECTION ( 'NONE',  ( 0.000000000000000000, -1.000000000000000000, 0.000000000000000000 ) ) ;
#5729 = DIRECTION ( 'NONE',  ( -0.000000000000000000, -0.000000000000000000, 1.000000000000000000 ) ) ;
#5730 = ORIENTED_EDGE ( 'NONE', *, *, #14063, .T. ) ;
#5731 = CARTESIAN_POINT ( 'NONE',  ( -3.339999999999998970, 4.090320309152158050E-16, -0.4621369752184044666 ) ) ;
#5732 = EDGE_CURVE ( 'NONE', #6920, #7913, #12588, .T. ) ;
#5733 = CARTESIAN_POINT ( 'NONE',  ( 0.5000000000000000000, -6.429618962271402616, -1.000000000000000000 ) ) ;
#5734 = AXIS2_PLACEMENT_3D ( 'NONE', #7407, #7252, #11893 ) ;
#5735 = DIRECTION ( 'NONE',  ( 0.000000000000000000, 0.000000000000000000, 1.000000000000000000 ) ) ;
#5736 = DIRECTION ( 'NONE',  ( 0.000000000000000000, 0.000000000000000000, 1.000000000000000000 ) ) ;
#5737 =( NAMED_UNIT ( * ) SI_UNIT ( $, .STERADIAN. ) SOLID_ANGLE_UNIT ( ) );
#5738 = VERTEX_POINT ( 'NONE', #5795 ) ;
#5739 = EDGE_CURVE ( 'NONE', #7944, #5923, #3099, .T. ) ;
#5740 = DIRECTION ( 'NONE',  ( 0.000000000000000000, 0.5000000000000018874, 0.8660254037844374864 ) ) ;
#5741 = ORIENTED_EDGE ( 'NONE', *, *, #8812, .F. ) ;
#5742 = EDGE_CURVE ( 'NONE', #11030, #4280, #8145, .T. ) ;
#5743 = ORIENTED_EDGE ( 'NONE', *, *, #2122, .T. ) ;
#5744 = DIRECTION ( 'NONE',  ( -0.9578262852211507639, 0.2873478855663477716, -0.000000000000000000 ) ) ;
#5745 = EDGE_CURVE ( 'NONE', #14275, #1794, #313, .T. ) ;
#5746 = DIRECTION ( 'NONE',  ( 1.148424442117023040E-15, -3.445273326351216045E-16, -1.000000000000000000 ) ) ;
#5747 = CARTESIAN_POINT ( 'NONE',  ( 2.500000000000000000, 2.357898499370431722, -2.818925648462311528E-15 ) ) ;
#5748 = CARTESIAN_POINT ( 'NONE',  ( 0.000000000000000000, 0.000000000000000000, 0.000000000000000000 ) ) ;
#5749 = DIRECTION ( 'NONE',  ( -0.8660254037844382635, 0.5000000000000005551, 0.000000000000000000 ) ) ;
#5750 = LINE ( 'NONE', #13797, #7800 ) ;
#5751 = CARTESIAN_POINT ( 'NONE',  ( 642.5000000000001137, 160.0000000000000284, 207.0000000000000000 ) ) ;
#5752 = ORIENTED_EDGE ( 'NONE', *, *, #34, .F. ) ;
#5753 = PLANE ( 'NONE',  #1860 ) ;
#5754 = CARTESIAN_POINT ( 'NONE',  ( -0.8808064505793390397, -6.997019658119205232, -5.875704392894199657 ) ) ;
#5755 = CARTESIAN_POINT ( 'NONE',  ( 6.367873360227559232, -5.773502691896264416, 0.000000000000000000 ) ) ;
#5756 = ORIENTED_EDGE ( 'NONE', *, *, #10016, .T. ) ;
#5757 = EDGE_CURVE ( 'NONE', #11781, #2369, #13838, .T. ) ;
#5758 = DIRECTION ( 'NONE',  ( 1.000000000000000000, 0.000000000000000000, 0.000000000000000000 ) ) ;
#5759 = ORIENTED_EDGE ( 'NONE', *, *, #4602, .F. ) ;
#5760 = EDGE_LOOP ( 'NONE', ( #164, #9742, #13383, #11176 ) ) ;
#5761 = CARTESIAN_POINT ( 'NONE',  ( 2.595115354961440524, -7.673029147243177306, -1.000000000000000000 ) ) ;
#5762 = PLANE ( 'NONE',  #4493 ) ;
#5763 = ADVANCED_FACE ( 'NONE', ( #3439 ), #1363, .F. ) ;
#5764 = CARTESIAN_POINT ( 'NONE',  ( 5.384454397937118664, 0.000000000000000000, -5.000000000000000000 ) ) ;
#5765 = PRODUCT_DEFINITION ( 'UNKNOWN', '', #515, #8118 ) ;
#5766 = DIRECTION ( 'NONE',  ( 1.000000000000000000, 0.000000000000000000, 0.000000000000000000 ) ) ;
#5767 = UNCERTAINTY_MEASURE_WITH_UNIT (LENGTH_MEASURE( 1.000000000000000082E-05 ), #8862, 'distance_accuracy_value', 'NONE');
#5768 = CARTESIAN_POINT ( 'NONE',  ( -3.309651814758565180, -5.455921364805393026, 0.000000000000000000 ) ) ;
#5769 = VERTEX_POINT ( 'NONE', #3516 ) ;
#5770 = CARTESIAN_POINT ( 'NONE',  ( -4.336808689942017736E-16, 7.505553499465137612, -0.8000000000000003775 ) ) ;
#5771 = FACE_OUTER_BOUND ( 'NONE', #10668, .T. ) ;
#5772 = LINE ( 'NONE', #6672, #12486 ) ;
#5773 = ORIENTED_EDGE ( 'NONE', *, *, #4319, .T. ) ;
#5774 = ORIENTED_EDGE ( 'NONE', *, *, #322, .F. ) ;
#5775 = CARTESIAN_POINT ( 'NONE',  ( 627.5000000000000000, 159.0182522957532285, 210.0000119999999981 ) ) ;
#5776 = DIRECTION ( 'NONE',  ( -0.2873478855663446629, -0.9578262852211516520, 0.000000000000000000 ) ) ;
#5777 = FACE_OUTER_BOUND ( 'NONE', #6392, .T. ) ;
#5778 = CARTESIAN_POINT ( 'NONE',  ( 4.000000000000000000, 0.8378280264232961239, -3.220590601395640018 ) ) ;
#5779 = EDGE_LOOP ( 'NONE', ( #7767, #4332, #10904, #979, #6233, #4387, #9042 ) ) ;
#5780 = EDGE_LOOP ( 'NONE', ( #4362, #8331, #3094, #4965 ) ) ;
#5781 = CARTESIAN_POINT ( 'NONE',  ( 610.0000000000001137, 191.1080398579018720, 187.0000000000000000 ) ) ;
#5782 = FACE_OUTER_BOUND ( 'NONE', #825, .T. ) ;
#5783 = EDGE_CURVE ( 'NONE', #4527, #9723, #247, .T. ) ;
#5784 = FACE_OUTER_BOUND ( 'NONE', #8055, .T. ) ;
#5785 = LINE ( 'NONE', #10287, #1361 ) ;
#5786 = CARTESIAN_POINT ( 'NONE',  ( 6.837824896291514243, 3.947820044545427454, -6.564402953523716278 ) ) ;
#5787 =( NAMED_UNIT ( * ) PLANE_ANGLE_UNIT ( ) SI_UNIT ( $, .RADIAN. ) );
#5788 = ORIENTED_EDGE ( 'NONE', *, *, #9279, .F. ) ;
#5789 = LINE ( 'NONE', #4551, #4011 ) ;
#5790 = ORIENTED_EDGE ( 'NONE', *, *, #10511, .T. ) ;
#5791 = ORIENTED_EDGE ( 'NONE', *, *, #2164, .T. ) ;
#5792 = CARTESIAN_POINT ( 'NONE',  ( 6.362366615495917976, 2.018765416951484593, -5.108861542006081002 ) ) ;
#5793 = ADVANCED_FACE ( 'NONE', ( #12431 ), #1297, .F. ) ;
#5794 = CARTESIAN_POINT ( 'NONE',  ( 0.2500000000000002220, 0.000000000000000000, 4.000000000000000000 ) ) ;
#5795 = CARTESIAN_POINT ( 'NONE',  ( 2.999999999999999112, -2.309401076758502480, -4.000000000000000000 ) ) ;
#5796 = ORIENTED_EDGE ( 'NONE', *, *, #4950, .T. ) ;
#5797 = DIRECTION ( 'NONE',  ( 1.000000000000000000, 0.000000000000000000, -0.000000000000000000 ) ) ;
#5798 = DIRECTION ( 'NONE',  ( -0.2873478855663419984, -0.9578262852211524292, -4.803849625782173317E-14 ) ) ;
#5799 = CARTESIAN_POINT ( 'NONE',  ( -1.860380241283027480, -6.431462466365327479, -0.1499059597315341996 ) ) ;
#5800 = DIRECTION ( 'NONE',  ( -0.000000000000000000, 0.000000000000000000, 1.000000000000000000 ) ) ;
#5801 =( NAMED_UNIT ( * ) SI_UNIT ( $, .STERADIAN. ) SOLID_ANGLE_UNIT ( ) );
#5802 = ORIENTED_EDGE ( 'NONE', *, *, #11544, .T. ) ;
#5803 = PLANE ( 'NONE',  #8714 ) ;
#5804 = ORIENTED_EDGE ( 'NONE', *, *, #9135, .T. ) ;
#5805 = VERTEX_POINT ( 'NONE', #3666 ) ;
#5806 = DIRECTION ( 'NONE',  ( 0.000000000000000000, 0.000000000000000000, 1.000000000000000000 ) ) ;
#5807 = PRODUCT_DEFINITION_SHAPE ( 'NONE', 'NONE',  #10810 ) ;
#5808 = EDGE_CURVE ( 'NONE', #13276, #1708, #2384, .T. ) ;
#5809 = CARTESIAN_POINT ( 'NONE',  ( 635.9940618270459254, 152.4999005938267658, -210.0000000000000000 ) ) ;
#5810 = FACE_OUTER_BOUND ( 'NONE', #14403, .T. ) ;
#5811 = CARTESIAN_POINT ( 'NONE',  ( 7.240873133980769261, 470.9098836221799047, -187.0000000000001990 ) ) ;
#5812 = CARTESIAN_POINT ( 'NONE',  ( -3.999999999999999112, 4.898587196589411843E-16, 3.469446951953614189E-15 ) ) ;
#5813 = DIRECTION ( 'NONE',  ( 0.000000000000000000, 0.000000000000000000, -1.000000000000000000 ) ) ;
#5814 = DIRECTION ( 'NONE',  ( 0.9578262852211513190, -0.2873478855663454401, 1.972152263052529951E-31 ) ) ;
#5815 = ORIENTED_EDGE ( 'NONE', *, *, #10063, .F. ) ;
#5816 = DIRECTION ( 'NONE',  ( 0.9578262852211514300, -0.2873478855663454956, 1.021394162290354552E-15 ) ) ;
#5817 = DIRECTION ( 'NONE',  ( -1.000000000000000000, -0.000000000000000000, -0.000000000000000000 ) ) ;
#5818 = CARTESIAN_POINT ( 'NONE',  ( 610.5828669213532294, 188.7537838752662935, 185.5093481647506906 ) ) ;
#5819 = ORIENTED_EDGE ( 'NONE', *, *, #5627, .F. ) ;
#5820 = CARTESIAN_POINT ( 'NONE',  ( 6.390820551024316565, -3.013776919160863876, 4.999999999999999112 ) ) ;
#5821 = VERTEX_POINT ( 'NONE', #13620 ) ;
#5822 = EDGE_LOOP ( 'NONE', ( #11306, #12689, #10139, #13309 ) ) ;
#5823 = DIRECTION ( 'NONE',  ( 0.2873478855663417764, 0.9578262852211525402, -6.938893903907204712E-15 ) ) ;
#5824 = EDGE_CURVE ( 'NONE', #6382, #14559, #11336, .T. ) ;
#5825 = VECTOR ( 'NONE', #10107, 1000.000000000000000 ) ;
#5827 = DIRECTION ( 'NONE',  ( 1.460819769243627131E-16, 0.000000000000000000, -1.000000000000000000 ) ) ;
#5826 = CIRCLE ( 'NONE', #1098, 5.100000000000000533 ) ;
#5828 = EDGE_CURVE ( 'NONE', #2732, #7703, #4662, .T. ) ;
#5829 = CARTESIAN_POINT ( 'NONE',  ( 610.8620436566991430, 188.5525593289318351, 169.9999999999999716 ) ) ;
#5830 = EDGE_CURVE ( 'NONE', #11091, #6727, #9117, .T. ) ;
#5831 = LINE ( 'NONE', #3994, #12906 ) ;
#5832 = ORIENTED_EDGE ( 'NONE', *, *, #1335, .T. ) ;
#5833 = MECHANICAL_DESIGN_GEOMETRIC_PRESENTATION_REPRESENTATION (  '', ( #3247 ), #4430 ) ;
#5834 = EDGE_CURVE ( 'NONE', #9095, #1716, #9196, .T. ) ;
#5835 = AXIS2_PLACEMENT_3D ( 'NONE', #8448, #8230, #12741 ) ;
#5836 = DIRECTION ( 'NONE',  ( 0.5000000000000013323, -0.8660254037844379305, 0.000000000000000000 ) ) ;
#5837 = DIRECTION ( 'NONE',  ( -0.2873478855663453846, -0.9578262852211513190, -0.000000000000000000 ) ) ;
#5838 = CARTESIAN_POINT ( 'NONE',  ( 0.000000000000000000, 0.000000000000000000, 0.000000000000000000 ) ) ;
#5839 = DIRECTION ( 'NONE',  ( 1.416419855379454792E-15, -4.619333907680102023E-16, -1.000000000000000000 ) ) ;
#5840 = ORIENTED_EDGE ( 'NONE', *, *, #7446, .T. ) ;
#5841 = ORIENTED_EDGE ( 'NONE', *, *, #6407, .F. ) ;
#5842 = CARTESIAN_POINT ( 'NONE',  ( 144.7991633467111683, 386.6211705227183870, 190.0000000000000000 ) ) ;
#5843 = DIRECTION ( 'NONE',  ( -0.000000000000000000, -0.000000000000000000, -1.000000000000000000 ) ) ;
#5844 = DIRECTION ( 'NONE',  ( 0.000000000000000000, 0.000000000000000000, 1.000000000000000000 ) ) ;
#5845 = CIRCLE ( 'NONE', #7493, 5.750000000000000000 ) ;
#5846 = AXIS2_PLACEMENT_3D ( 'NONE', #12044, #5488, #6374 ) ;
#5847 = EDGE_CURVE ( 'NONE', #2902, #7138, #863, .T. ) ;
#5848 = ORIENTED_EDGE ( 'NONE', *, *, #10511, .F. ) ;
#5849 = EDGE_LOOP ( 'NONE', ( #6138, #1298, #4760, #758 ) ) ;
#5850 = CARTESIAN_POINT ( 'NONE',  ( 6.534533895392296010, -2.951347675328738873, -5.111884124469658452 ) ) ;
#5851 = CARTESIAN_POINT ( 'NONE',  ( 2.837346585668845567, -6.232092946297389524, -6.171287963165198676 ) ) ;
#5852 = LINE ( 'NONE', #5939, #11264 ) ;
#5853 = FACE_OUTER_BOUND ( 'NONE', #11638, .T. ) ;
#5854 = DIRECTION ( 'NONE',  ( -0.000000000000000000, -0.000000000000000000, -1.000000000000000000 ) ) ;
#5855 = SHAPE_REPRESENTATION_RELATIONSHIP ( 'NONE' , 'NONE' ,  #12910, #10030 ) ;
#5856 = VERTEX_POINT ( 'NONE', #11469 ) ;
#5857 = VECTOR ( 'NONE', #12223, 1000.000000000000000 ) ;
#5858 = DIRECTION ( 'NONE',  ( 0.9578262852211504308, -0.2873478855663483267, 0.000000000000000000 ) ) ;
#5859 = AXIS2_PLACEMENT_3D ( 'NONE', #2372, #8057, #2448 ) ;
#5860 = ORIENTED_EDGE ( 'NONE', *, *, #4345, .T. ) ;
#5861 = EDGE_LOOP ( 'NONE', ( #1868, #8886, #6528, #7936 ) ) ;
#5862 = CARTESIAN_POINT ( 'NONE',  ( 6.204471256524902500, -0.9979289516705972529, -5.000000000000444089 ) ) ;
#5863 = EDGE_CURVE ( 'NONE', #10556, #4981, #3475, .T. ) ;
#5864 = VECTOR ( 'NONE', #5245, 1000.000000000000114 ) ;
#5865 = EDGE_CURVE ( 'NONE', #8019, #10404, #11407, .T. ) ;
#5866 = DIRECTION ( 'NONE',  ( -0.000000000000000000, -0.000000000000000000, 1.000000000000000000 ) ) ;
#5867 = B_SPLINE_CURVE_WITH_KNOTS ( 'NONE', 3,
 ( #13537, #71, #1202, #7986, #6958, #11653 ),
 .UNSPECIFIED., .F., .F.,
 ( 4, 2, 4 ),
 ( 0.002452478801916376308, 0.003676905084148007850, 0.004901331366379639391 ),
 .UNSPECIFIED. ) ;
#5868 = CARTESIAN_POINT ( 'NONE',  ( 2.500000000000000000, -1.178949249685218748, -2.041999999999998039 ) ) ;
#5869 = CIRCLE ( 'NONE', #14126, 6.500000000000000888 ) ;
#5870 = ORIENTED_EDGE ( 'NONE', *, *, #10207, .T. ) ;
#5871 = FACE_OUTER_BOUND ( 'NONE', #4443, .T. ) ;
#5872 = DIRECTION ( 'NONE',  ( 0.9578262852211514300, -0.2873478855663454401, 2.126801590887410810E-15 ) ) ;
#5873 = PLANE ( 'NONE',  #3951 ) ;
#5874 =( NAMED_UNIT ( * ) PLANE_ANGLE_UNIT ( ) SI_UNIT ( $, .RADIAN. ) );
#5875 = ORIENTED_EDGE ( 'NONE', *, *, #14481, .F. ) ;
#5876 = CIRCLE ( 'NONE', #14133, 4.799999999999968736 ) ;
#5877 = DIRECTION ( 'NONE',  ( 1.000000000000000000, 0.000000000000000000, 0.000000000000000000 ) ) ;
#5878 = ORIENTED_EDGE ( 'NONE', *, *, #5250, .T. ) ;
#5879 = CIRCLE ( 'NONE', #5172, 2.649999999999985700 ) ;
#5880 = AXIS2_PLACEMENT_3D ( 'NONE', #2324, #1007, #10015 ) ;
#5881 = ORIENTED_EDGE ( 'NONE', *, *, #4409, .T. ) ;
#5882 = CARTESIAN_POINT ( 'NONE',  ( 446.3084422793565409, 264.0194060144110608, 187.0000000000000000 ) ) ;
#5883 = CARTESIAN_POINT ( 'NONE',  ( 0.000000000000000000, 7.654042494670957606E-16, -6.250000000000000000 ) ) ;
#5884 = VECTOR ( 'NONE', #6082, 1000.000000000000227 ) ;
#5885 = LINE ( 'NONE', #10395, #1444 ) ;
#5886 = ORIENTED_EDGE ( 'NONE', *, *, #2310, .F. ) ;
#5887 = DIRECTION ( 'NONE',  ( 0.000000000000000000, 0.000000000000000000, 1.000000000000000000 ) ) ;
#5888 = CIRCLE ( 'NONE', #9899, 2.041999999999999815 ) ;
#5889 = VECTOR ( 'NONE', #2849, 1000.000000000000000 ) ;
#5890 = DIRECTION ( 'NONE',  ( 0.000000000000000000, -1.000000000000000000, 6.965275210156238168E-15 ) ) ;
#5891 = DIRECTION ( 'NONE',  ( 0.2873478855663439413, 0.9578262852211518741, 0.000000000000000000 ) ) ;
#5892 = CARTESIAN_POINT ( 'NONE',  ( 0.3108895250736378735, -2.416698868092693075, -5.000000000000000000 ) ) ;
#5893 = EDGE_CURVE ( 'NONE', #2224, #1364, #10455, .T. ) ;
#5894 = ORIENTED_EDGE ( 'NONE', *, *, #5824, .T. ) ;
#5895 = FACE_OUTER_BOUND ( 'NONE', #517, .T. ) ;
#5896 = DIRECTION ( 'NONE',  ( -0.000000000000000000, -0.000000000000000000, -1.000000000000000000 ) ) ;
#5897 = CARTESIAN_POINT ( 'NONE',  ( 6.495567275914614136, 2.917443832165055539, -5.053160945538337501 ) ) ;
#5898 = CONTEXT_DEPENDENT_SHAPE_REPRESENTATION ( #13105, #7120 ) ;
#5899 = ORIENTED_EDGE ( 'NONE', *, *, #5347, .T. ) ;
#5900 = AXIS2_PLACEMENT_3D ( 'NONE', #13011, #10868, #660 ) ;
#5901 = CIRCLE ( 'NONE', #10148, 4.799999999999968736 ) ;
#5902 = CARTESIAN_POINT ( 'NONE',  ( 6.212075932873402984, -2.040040303548923628, 4.999999999999999112 ) ) ;
#5903 = VERTEX_POINT ( 'NONE', #8223 ) ;
#5904 = ORIENTED_EDGE ( 'NONE', *, *, #1954, .T. ) ;
#5905 =( NAMED_UNIT ( * ) PLANE_ANGLE_UNIT ( ) SI_UNIT ( $, .RADIAN. ) );
#5906 = LINE ( 'NONE', #5981, #9197 ) ;
#5907 = AXIS2_PLACEMENT_3D ( 'NONE', #14280, #982, #9995 ) ;
#5908 = CARTESIAN_POINT ( 'NONE',  ( 6.436591462021373999, -2.894509378375943243, 5.013437306331755217 ) ) ;
#5909 = AXIS2_PLACEMENT_3D ( 'NONE', #13743, #11441, #8053 ) ;
#5910 = LINE ( 'NONE', #5829, #7803 ) ;
#5911 = AXIS2_PLACEMENT_3D ( 'NONE', #6575, #14539, #4431 ) ;
#5912 = PRODUCT_DEFINITION_CONTEXT ( 'detailed design', #13660, 'design' ) ;
#5913 = DIRECTION ( 'NONE',  ( 0.9578262852211513190, -0.2873478855663453291, 0.000000000000000000 ) ) ;
#5914 = EDGE_CURVE ( 'NONE', #10093, #14518, #2633, .T. ) ;
#5915 = ORIENTED_EDGE ( 'NONE', *, *, #13577, .F. ) ;
#5916 = AXIS2_PLACEMENT_3D ( 'NONE', #14434, #12126, #2987 ) ;
#5917 = CARTESIAN_POINT ( 'NONE',  ( -2.690931834596280936, 5.951943280390038282, 1.006275141338108408E-15 ) ) ;
#5918 = DIRECTION ( 'NONE',  ( -1.000000000000000000, -0.000000000000000000, -0.000000000000000000 ) ) ;
#5919 = DIRECTION ( 'NONE',  ( 0.000000000000000000, 0.000000000000000000, 1.000000000000000000 ) ) ;
#5920 = EDGE_CURVE ( 'NONE', #3289, #14092, #6174, .T. ) ;
#5921 = CARTESIAN_POINT ( 'NONE',  ( 6.367873360227556567, 2.886751345948125547, 4.999999999999999112 ) ) ;
#5922 = ORIENTED_EDGE ( 'NONE', *, *, #544, .F. ) ;
#5923 = VERTEX_POINT ( 'NONE', #473 ) ;
#5924 = CIRCLE ( 'NONE', #7101, 4.199999999999981526 ) ;
#5925 = DIRECTION ( 'NONE',  ( -1.000000000000000000, -0.000000000000000000, -0.000000000000000000 ) ) ;
#5926 = CARTESIAN_POINT ( 'NONE',  ( 641.0000000000000000, 154.0000000000000568, -187.5000000000000000 ) ) ;
#5927 = CIRCLE ( 'NONE', #3073, 3.399999999999999911 ) ;
#5928 = EDGE_CURVE ( 'NONE', #793, #5539, #11239, .T. ) ;
#5929 = DIRECTION ( 'NONE',  ( 0.9578262852211513190, -0.2873478855663453846, -8.575812866481462478E-17 ) ) ;
#5930 = VECTOR ( 'NONE', #11701, 1000.000000000000114 ) ;
#5931 = ADVANCED_FACE ( 'NONE', ( #12880 ), #6238, .F. ) ;
#5932 = COLOUR_RGB ( '',1.000000000000000000, 0.9490196078431372140, 0.9098039215686274384 ) ;
#5933 = SHAPE_REPRESENTATION ( 'circlip for shafts normal_din_Circlip DIN 471 - 10 x 1', ( #9440 ), #5461 ) ;
#5934 = ORIENTED_EDGE ( 'NONE', *, *, #13940, .F. ) ;
#5935 = CONICAL_SURFACE ( 'NONE', #6880, 4.000000000000000000, 0.8911886515913786111 ) ;
#5936 = VERTEX_POINT ( 'NONE', #13925 ) ;
#5937 = PLANE ( 'NONE',  #8776 ) ;
#5938 = FACE_BOUND ( 'NONE', #4725, .T. ) ;
#5939 = CARTESIAN_POINT ( 'NONE',  ( 142.4540310085880606, 355.9707293956415697, -210.0000000000000000 ) ) ;
#5940 = DIRECTION ( 'NONE',  ( -0.9578262852211513190, 0.2873478855663453846, 0.000000000000000000 ) ) ;
#5941 =( NAMED_UNIT ( * ) PLANE_ANGLE_UNIT ( ) SI_UNIT ( $, .RADIAN. ) );
#5942 = ORIENTED_EDGE ( 'NONE', *, *, #13987, .F. ) ;
#5943 =( GEOMETRIC_REPRESENTATION_CONTEXT ( 3 ) GLOBAL_UNCERTAINTY_ASSIGNED_CONTEXT ( ( #10770 ) ) GLOBAL_UNIT_ASSIGNED_CONTEXT ( ( #7119, #13025, #7334 ) ) REPRESENTATION_CONTEXT ( 'NONE', 'WORKASPACE' ) );
#5944 = DIRECTION ( 'NONE',  ( 0.000000000000000000, 0.000000000000000000, 1.000000000000000000 ) ) ;
#5945 = ORIENTED_EDGE ( 'NONE', *, *, #9374, .T. ) ;
#5946 = ORIENTED_EDGE ( 'NONE', *, *, #10054, .F. ) ;
#5947 = DIRECTION ( 'NONE',  ( 2.022127743178574844E-16, 3.939404418192334771E-15, 1.000000000000000000 ) ) ;
#5948 = ADVANCED_FACE ( 'NONE', ( #12813 ), #9605, .T. ) ;
#5949 = EDGE_CURVE ( 'NONE', #12031, #556, #6306, .T. ) ;
#5950 = AXIS2_PLACEMENT_3D ( 'NONE', #3841, #1753, #7438 ) ;
#5951 = EDGE_CURVE ( 'NONE', #10586, #14514, #2489, .T. ) ;
#5952 = DIRECTION ( 'NONE',  ( 1.000000000000000000, 0.000000000000000000, 0.000000000000000000 ) ) ;
#5953 = DIRECTION ( 'NONE',  ( 0.000000000000000000, -0.5000000000000009992, -0.8660254037844380415 ) ) ;
#5954 = PRODUCT_DEFINITION_FORMATION_WITH_SPECIFIED_SOURCE ( 'ANY', '', #13474, .NOT_KNOWN. ) ;
#5955 = ORIENTED_EDGE ( 'NONE', *, *, #4058, .F. ) ;
#5956 = DIRECTION ( 'NONE',  ( 0.000000000000000000, 0.000000000000000000, -1.000000000000000000 ) ) ;
#5957 = FACE_OUTER_BOUND ( 'NONE', #9825, .T. ) ;
#5958 = CARTESIAN_POINT ( 'NONE',  ( 6.534838248920896930, -2.951765777552407766, 5.112608298763836601 ) ) ;
#5959 = LINE ( 'NONE', #2019, #529 ) ;
#5960 = AXIS2_PLACEMENT_3D ( 'NONE', #9741, #3166, #13194 ) ;
#5961 = VERTEX_POINT ( 'NONE', #8439 ) ;
#5962 = AXIS2_PLACEMENT_3D ( 'NONE', #5406, #2000, #4096 ) ;
#5963 = CARTESIAN_POINT ( 'NONE',  ( 706.6446721788141758, 159.8177707722969956, 177.6000000000005627 ) ) ;
#5964 = EDGE_LOOP ( 'NONE', ( #12286, #9782, #13998, #1221 ) ) ;
#5965 = VERTEX_POINT ( 'NONE', #5003 ) ;
#5966 = CARTESIAN_POINT ( 'NONE',  ( 635.0000000000000000, 160.0000000000000284, 210.0000000000000000 ) ) ;
#5967 = CARTESIAN_POINT ( 'NONE',  ( -4.137823196307924351E-15, 4.821944789745366222, -1.648146632869000427 ) ) ;
#5968 = CARTESIAN_POINT ( 'NONE',  ( 142.4540310085880606, 355.9707293956415697, -187.0000000000000000 ) ) ;
#5969 = ORIENTED_EDGE ( 'NONE', *, *, #4207, .T. ) ;
#5970 = CARTESIAN_POINT ( 'NONE',  ( 455.5035746174796714, 294.6698471414878782, -190.0000000000000568 ) ) ;
#5971 = CARTESIAN_POINT ( 'NONE',  ( -6.500000000000000888, 0.000000000000000000, 0.000000000000000000 ) ) ;
#5972 = DIRECTION ( 'NONE',  ( -0.9578262852211513190, 0.2873478855663454956, -1.110223024625156540E-15 ) ) ;
#5973 = CARTESIAN_POINT ( 'NONE',  ( 650.0000000000000000, 145.0000000000000568, -210.0000000000000000 ) ) ;
#5974 = ORIENTED_EDGE ( 'NONE', *, *, #8181, .T. ) ;
#5975 = DIRECTION ( 'NONE',  ( 1.000000000000000000, 0.000000000000000000, 0.000000000000000000 ) ) ;
#5976 = FILL_AREA_STYLE ('',( #11578 ) ) ;
#5977 = ORIENTED_EDGE ( 'NONE', *, *, #4486, .T. ) ;
#5978 = CARTESIAN_POINT ( 'NONE',  ( 6.095484975317565279, -1.047622383848427985, 4.999999999999999112 ) ) ;
#5979 = ORIENTED_EDGE ( 'NONE', *, *, #11276, .T. ) ;
#5980 = ORIENTED_EDGE ( 'NONE', *, *, #11528, .T. ) ;
#5981 = CARTESIAN_POINT ( 'NONE',  ( 21.00000000000000355, 0.000000000000000000, 2.055000000000000160 ) ) ;
#5982 = CARTESIAN_POINT ( 'NONE',  ( 3.679171394226031122, 2.494631558665830973, -0.3503314178412474389 ) ) ;
#5983 = EDGE_CURVE ( 'NONE', #2291, #8153, #11705, .T. ) ;
#5984 = EDGE_CURVE ( 'NONE', #12898, #1836, #10779, .T. ) ;
#5985 = CARTESIAN_POINT ( 'NONE',  ( 0.000000000000000000, 0.000000000000000000, 0.000000000000000000 ) ) ;
#5986 = CARTESIAN_POINT ( 'NONE',  ( 139.8040310085880833, 355.9707293956415697, 187.0000000000000000 ) ) ;
#5987 = ORIENTED_EDGE ( 'NONE', *, *, #5384, .F. ) ;
#5988 = LINE ( 'NONE', #11659, #4182 ) ;
#5989 = CARTESIAN_POINT ( 'NONE',  ( -1.828356344711647319, -3.563200125723192002, -1.076197711133951296E-14 ) ) ;
#5990 = CARTESIAN_POINT ( 'NONE',  ( 148.9991633467111569, 386.6211705227183870, 178.5000000000000568 ) ) ;
#5991 = DIRECTION ( 'NONE',  ( 0.000000000000000000, 0.000000000000000000, 1.000000000000000000 ) ) ;
#5992 = VECTOR ( 'NONE', #6196, 1000.000000000000000 ) ;
#5993 = EDGE_LOOP ( 'NONE', ( #6368, #894, #11400, #8070 ) ) ;
#5994 = VERTEX_POINT ( 'NONE', #10811 ) ;
#5995 = CARTESIAN_POINT ( 'NONE',  ( 627.5000000000000000, 160.0000000000000284, 210.0000059999999849 ) ) ;
#5996 = DIRECTION ( 'NONE',  ( 0.000000000000000000, 0.000000000000000000, 1.000000000000000000 ) ) ;
#5997 = CARTESIAN_POINT ( 'NONE',  ( 610.0000000000000000, 227.4403065089105951, 187.0000000000000000 ) ) ;
#5998 = ADVANCED_FACE ( 'NONE', ( #9635 ), #13036, .T. ) ;
#5999 = VERTEX_POINT ( 'NONE', #8375 ) ;
#6000 = CARTESIAN_POINT ( 'NONE',  ( -8.505790995054779202, 418.4210031920615620, -184.7999999999999829 ) ) ;
#6001 = CARTESIAN_POINT ( 'NONE',  ( 629.0000000000000000, 166.0000000000000284, 187.5000000000000000 ) ) ;
#6002 = FACE_OUTER_BOUND ( 'NONE', #1641, .T. ) ;
#6003 = ADVANCED_FACE ( 'NONE', ( #3822 ), #12901, .T. ) ;
#6004 = DIRECTION ( 'NONE',  ( -1.000000000000000000, 0.000000000000000000, 0.000000000000000000 ) ) ;
#6005 = DIRECTION ( 'NONE',  ( -0.9578262852211514300, 0.2873478855663454401, 0.000000000000000000 ) ) ;
#6006 = CARTESIAN_POINT ( 'NONE',  ( 703.1581845006096501, 166.2926764603917036, -177.6000000000005059 ) ) ;
#6007 = ORIENTED_EDGE ( 'NONE', *, *, #8101, .F. ) ;
#6008 = FACE_OUTER_BOUND ( 'NONE', #5712, .T. ) ;
#6009 = VERTEX_POINT ( 'NONE', #11686 ) ;
#6010 = ORIENTED_EDGE ( 'NONE', *, *, #13587, .T. ) ;
#6011 = LINE ( 'NONE', #5070, #13941 ) ;
#6012 = EDGE_CURVE ( 'NONE', #3424, #6009, #8166, .T. ) ;
#6013 = CARTESIAN_POINT ( 'NONE',  ( 33.50000000000000000, 0.000000000000000000, 0.000000000000000000 ) ) ;
#6014 = CARTESIAN_POINT ( 'NONE',  ( 708.1388811837593948, 164.7984674554458593, -182.7999999999998977 ) ) ;
#6015 = DIRECTION ( 'NONE',  ( -0.4113766427172327877, 0.9114654452181378819, 0.000000000000000000 ) ) ;
#6016 = EDGE_LOOP ( 'NONE', ( #1276, #9249, #13479 ) ) ;
#6017 = EDGE_CURVE ( 'NONE', #7658, #9573, #1662, .T. ) ;
#6018 = DIRECTION ( 'NONE',  ( 0.9578262852211513190, -0.2873478855663453846, 0.000000000000000000 ) ) ;
#6019 = DIRECTION ( 'NONE',  ( 0.000000000000000000, 0.000000000000000000, -1.000000000000000000 ) ) ;
#6020 = EDGE_CURVE ( 'NONE', #11328, #8163, #8063, .T. ) ;
#6021 = CARTESIAN_POINT ( 'NONE',  ( -1.390230914382372118, -4.043987460488664532, -3.502507215260523665 ) ) ;
#6022 = CARTESIAN_POINT ( 'NONE',  ( -20.63749999999999574, 0.000000000000000000, 0.000000000000000000 ) ) ;
#6023 = ORIENTED_EDGE ( 'NONE', *, *, #2654, .F. ) ;
#6024 = EDGE_CURVE ( 'NONE', #5143, #488, #5329, .T. ) ;
#6025 = DIRECTION ( 'NONE',  ( -1.000000000000000000, 0.000000000000000000, 0.000000000000000000 ) ) ;
#6026 = ORIENTED_EDGE ( 'NONE', *, *, #4324, .T. ) ;
#6027 = DIRECTION ( 'NONE',  ( 1.000000000000000000, 0.000000000000000000, 0.000000000000000000 ) ) ;
#6028 =( REPRESENTATION_RELATIONSHIP ('NONE','NONE', #2822, #6779 ) REPRESENTATION_RELATIONSHIP_WITH_TRANSFORMATION ( #11854 )SHAPE_REPRESENTATION_RELATIONSHIP( ) );
#6029 = CARTESIAN_POINT ( 'NONE',  ( -4.000000000000000000, -2.309401076758515803, -0.4999999999999995559 ) ) ;
#6030 = CARTESIAN_POINT ( 'NONE',  ( 8.331345277524542681, 0.000000000000000000, -7.381345277524544279 ) ) ;
#6031 = ORIENTED_EDGE ( 'NONE', *, *, #3226, .T. ) ;
#6032 = LINE ( 'NONE', #10532, #5000 ) ;
#6033 = CARTESIAN_POINT ( 'NONE',  ( -4.000000000000000000, -2.309401076758515803, -0.4999999999999995559 ) ) ;
#6034 = DIRECTION ( 'NONE',  ( -0.7071067811865530128, 0.000000000000000000, 0.7071067811865421326 ) ) ;
#6035 = CARTESIAN_POINT ( 'NONE',  ( -6.500000000000000000, -3.752776749732573247, -0.8000000000000003775 ) ) ;
#6036 = VERTEX_POINT ( 'NONE', #8197 ) ;
#6037 = CARTESIAN_POINT ( 'NONE',  ( -4.000000000000000000, 1.700094919196744270, -3.320312364301766017 ) ) ;
#6038 = DIRECTION ( 'NONE',  ( 0.000000000000000000, 0.000000000000000000, 1.000000000000000000 ) ) ;
#6039 = ORIENTED_EDGE ( 'NONE', *, *, #3856, .F. ) ;
#6040 = DIRECTION ( 'NONE',  ( -0.000000000000000000, 1.000000000000000000, -1.224646799147353207E-16 ) ) ;
#6041 = ORIENTED_EDGE ( 'NONE', *, *, #1312, .F. ) ;
#6042 = ORIENTED_EDGE ( 'NONE', *, *, #8563, .T. ) ;
#6043 = DIRECTION ( 'NONE',  ( 0.000000000000000000, 0.000000000000000000, -1.000000000000000000 ) ) ;
#6044 = CARTESIAN_POINT ( 'NONE',  ( 0.000000000000000000, 0.000000000000000000, -1.000000000000000000 ) ) ;
#6045 = ADVANCED_FACE ( 'NONE', ( #294 ), #13366, .T. ) ;
#6046 = CARTESIAN_POINT ( 'NONE',  ( 455.5035746174796714, 294.6698471414878782, -190.0000000000000000 ) ) ;
#6047 = CARTESIAN_POINT ( 'NONE',  ( 3.999999999999998224, 2.472263674411418588, -3.687027874309861897 ) ) ;
#6048 = EDGE_CURVE ( 'NONE', #7703, #11833, #13837, .T. ) ;
#6049 = PRODUCT ( 'sliding channel', 'sliding channel', '', ( #5392 ) ) ;
#6050 = CARTESIAN_POINT ( 'NONE',  ( 610.0000000000000000, 227.4403065089105951, 210.0000000000000000 ) ) ;
#6051 = UNCERTAINTY_MEASURE_WITH_UNIT (LENGTH_MEASURE( 1.000000000000000082E-05 ), #12580, 'distance_accuracy_value', 'NONE');
#6052 = CARTESIAN_POINT ( 'NONE',  ( 6.837824896291514243, -3.947820044545437224, -6.564402953523717166 ) ) ;
#6053 = VERTEX_POINT ( 'NONE', #3716 ) ;
#6054 = CARTESIAN_POINT ( 'NONE',  ( 1.600000000000000089, 0.000000000000000000, 0.000000000000000000 ) ) ;
#6055 = CARTESIAN_POINT ( 'NONE',  ( 615.0000000000000000, 160.0000000000000284, 187.5000000000000000 ) ) ;
#6056 = DIRECTION ( 'NONE',  ( 0.000000000000000000, 0.000000000000000000, -1.000000000000000000 ) ) ;
#6057 = B_SPLINE_CURVE_WITH_KNOTS ( 'NONE', 3,
 ( #6384, #14494, #4381, #5420, #8875 ),
 .UNSPECIFIED., .F., .F.,
 ( 4, 1, 4 ),
 ( 0.000000000000000000, 0.002309401076758506657, 0.004618802153517013315 ),
 .UNSPECIFIED. ) ;
#6058 = AXIS2_PLACEMENT_3D ( 'NONE', #14186, #6502, #5258 ) ;
#6059 = DIRECTION ( 'NONE',  ( -0.2873478855663453291, -0.9578262852211513190, 0.000000000000000000 ) ) ;
#6060 = ADVANCED_FACE ( 'NONE', ( #6955 ), #2516, .F. ) ;
#6061 = CIRCLE ( 'NONE', #8414, 5.199999999999715961 ) ;
#6062 = ORIENTED_EDGE ( 'NONE', *, *, #10983, .T. ) ;
#6063 = ORIENTED_EDGE ( 'NONE', *, *, #3510, .F. ) ;
#6064 = CARTESIAN_POINT ( 'NONE',  ( 6.815830331203685866, 1.228021141713631082E-13, -6.171384342982610960 ) ) ;
#6065 = CARTESIAN_POINT ( 'NONE',  ( -10.00000000000002487, 371.6790804732684705, 184.8000000000000114 ) ) ;
#6066 = B_SPLINE_CURVE_WITH_KNOTS ( 'NONE', 3,
 ( #13049, #11497, #701, #6934, #1323, #12614, #9143, #11853, #558, #2436, #5146, #5818, #14152, #7277, #13649, #3545 ),
 .UNSPECIFIED., .F., .F.,
 ( 4, 2, 2, 2, 2, 2, 2, 4 ),
 ( 8.777083671441753062E-17, 0.0009429092714760194203, 0.001414363907214010374, 0.001885818542952001327, 0.002357273178689992064, 0.002828727814427983017, 0.003300182450165973971, 0.003771637085903964924 ),
 .UNSPECIFIED. ) ;
#6067 = CARTESIAN_POINT ( 'NONE',  ( 4.799999999999999822, 0.000000000000000000, -1.000000000000000000 ) ) ;
#6068 = CARTESIAN_POINT ( 'NONE',  ( 139.8040310085880833, 355.9707293956415697, -210.0000000000000000 ) ) ;
#6069 = B_SPLINE_CURVE_WITH_KNOTS ( 'NONE', 3,
 ( #14085, #5156, #2714, #8468, #11923, #6033 ),
 .UNSPECIFIED., .F., .F.,
 ( 4, 2, 4 ),
 ( 0.002365888236228001588, 0.003551327329835089319, 0.004736766423442177049 ),
 .UNSPECIFIED. ) ;
#6071 = VERTEX_POINT ( 'NONE', #5842 ) ;
#6070 = VECTOR ( 'NONE', #5162, 1000.000000000000000 ) ;
#6072 = CIRCLE ( 'NONE', #7484, 2.100000000000000089 ) ;
#6073 = EDGE_CURVE ( 'NONE', #10509, #10228, #13819, .T. ) ;
#6074 = CARTESIAN_POINT ( 'NONE',  ( 590.0000000000000000, -9.999999999999941380, -190.0000000000000000 ) ) ;
#6075 = CARTESIAN_POINT ( 'NONE',  ( -8.505790995054926640, 376.6597771564183859, 187.0000000000000000 ) ) ;
#6076 = CARTESIAN_POINT ( 'NONE',  ( -6.837824896291515131, -3.947820044545435447, -6.564402953523717166 ) ) ;
#6077 = DIRECTION ( 'NONE',  ( -1.000000000000000000, -0.000000000000000000, -0.000000000000000000 ) ) ;
#6078 = FACE_OUTER_BOUND ( 'NONE', #9353, .T. ) ;
#6079 = CARTESIAN_POINT ( 'NONE',  ( -2.837346585668847787, 6.232092946297378866, -6.171287963165196899 ) ) ;
#6080 = EDGE_CURVE ( 'NONE', #10070, #14108, #13963, .T. ) ;
#6081 = ORIENTED_EDGE ( 'NONE', *, *, #6669, .T. ) ;
#6082 = DIRECTION ( 'NONE',  ( -0.2873478855663454401, -0.9578262852211513190, -4.930380657631323784E-32 ) ) ;
#6083 = EDGE_LOOP ( 'NONE', ( #6010, #14058, #10563, #5875 ) ) ;
#6084 = EDGE_LOOP ( 'NONE', ( #11470, #14535, #11003, #8827, #13799, #3144, #2964 ) ) ;
#6085 = CARTESIAN_POINT ( 'NONE',  ( 133.6739427831727198, 370.3381236739588758, -210.0000000000000000 ) ) ;
#6086 = AXIS2_PLACEMENT_3D ( 'NONE', #9764, #810, #6146 ) ;
#6087 = VECTOR ( 'NONE', #5121, 1000.000000000000000 ) ;
#6088 = LINE ( 'NONE', #14134, #11558 ) ;
#6089 = B_SPLINE_CURVE_WITH_KNOTS ( 'NONE', 3,
 ( #9622, #4161, #12116, #4102, #14123, #13094 ),
 .UNSPECIFIED., .F., .F.,
 ( 4, 2, 4 ),
 ( -3.640115492407174633E-06, 0.0002066546034003413743, 0.0004169493222930899571 ),
 .UNSPECIFIED. ) ;
#6090 = CARTESIAN_POINT ( 'NONE',  ( 0.000000000000000000, 0.000000000000000000, -5.000000000000000000 ) ) ;
#6091 = DIRECTION ( 'NONE',  ( 0.2873478855663453846, 0.9578262852211513190, 0.000000000000000000 ) ) ;
#6092 = ORIENTED_EDGE ( 'NONE', *, *, #11301, .F. ) ;
#6093 = CARTESIAN_POINT ( 'NONE',  ( 455.5035746174796714, 294.6698471414878782, 190.0000000000000000 ) ) ;
#6094 = DIRECTION ( 'NONE',  ( -0.9578262852211512079, 0.2873478855663461617, -1.110223024625162260E-15 ) ) ;
#6095 = AXIS2_PLACEMENT_3D ( 'NONE', #9960, #14462, #12376 ) ;
#6096 = VECTOR ( 'NONE', #12046, 1000.000000000000114 ) ;
#6097 = VECTOR ( 'NONE', #5105, 1000.000000000000000 ) ;
#6098 = DIRECTION ( 'NONE',  ( 0.000000000000000000, 0.000000000000000000, -1.000000000000000000 ) ) ;
#6099 = DIRECTION ( 'NONE',  ( 0.000000000000000000, 0.000000000000000000, -1.000000000000000000 ) ) ;
#6100 = SURFACE_STYLE_FILL_AREA ( #12660 ) ;
#6101 = EDGE_CURVE ( 'NONE', #4614, #13147, #2453, .T. ) ;
#6102 = ORIENTED_EDGE ( 'NONE', *, *, #6483, .F. ) ;
#6103 = LINE ( 'NONE', #5963, #1640 ) ;
#6104 =( BOUNDED_SURFACE ( )  B_SPLINE_SURFACE ( 3, 2, ( 
 ( #6860, #12456, #11212 ),
 ( #2495, #7833, #12385 ),
 ( #2269, #6997, #11496 ),
 ( #5685, #4427, #13512 ),
 ( #5754, #6780, #8109 ),
 ( #11285, #1391, #12613 ) ),
 .UNSPECIFIED., .F., .F., .T. ) 
 B_SPLINE_SURFACE_WITH_KNOTS ( ( 4, 2, 4 ),
 ( 3, 3 ),
 ( 0.003190620565844225990, 0.007281897438794491043, 0.01137317431174475653 ),
 ( 0.000000000000000000, 1.000000000000000000 ),
 .UNSPECIFIED. ) 
 GEOMETRIC_REPRESENTATION_ITEM ( )  RATIONAL_B_SPLINE_SURFACE ( (
 ( 1.000000000000000000, 0.8047731410850402778, 1.000000000000000000),
 ( 1.000000000000000000, 0.8125552299156234559, 1.000000000000000000),
 ( 1.000000000000000000, 0.8191520442889865805, 1.000000000000000000),
 ( 1.000000000000000000, 0.8191520442889865805, 1.000000000000000000),
 ( 1.000000000000000000, 0.8125552299156227898, 1.000000000000000000),
 ( 1.000000000000000000, 0.8047731410850399447, 1.000000000000000000) ) ) 
 REPRESENTATION_ITEM ( '' )  SURFACE ( )  );
#6105 = ORIENTED_EDGE ( 'NONE', *, *, #6303, .F. ) ;
#6106 = EDGE_CURVE ( 'NONE', #5692, #7390, #4677, .T. ) ;
#6107 = CARTESIAN_POINT ( 'NONE',  ( 637.5000000000000000, 160.0000000000000284, -233.5000000000000000 ) ) ;
#6108 = AXIS2_PLACEMENT_3D ( 'NONE', #9579, #6526, #2646 ) ;
#6109 = EDGE_CURVE ( 'NONE', #8256, #10297, #11522, .T. ) ;
#6110 = AXIS2_PLACEMENT_3D ( 'NONE', #11213, #9076, #4428 ) ;
#6111 = DIRECTION ( 'NONE',  ( 1.000000000000000000, 0.000000000000000000, 0.000000000000000000 ) ) ;
#6112 = DIRECTION ( 'NONE',  ( 0.2873478855663454401, 0.9578262852211513190, 0.000000000000000000 ) ) ;
#6113 = EDGE_CURVE ( 'NONE', #8728, #5554, #11665, .T. ) ;
#6114 = ORIENTED_EDGE ( 'NONE', *, *, #8516, .F. ) ;
#6115 = CARTESIAN_POINT ( 'NONE',  ( 610.0417734222098716, 190.7948035559919333, 187.0000000000000284 ) ) ;
#6116 = VECTOR ( 'NONE', #2350, 1000.000000000000114 ) ;
#6117 = DIRECTION ( 'NONE',  ( -1.000000000000000000, 0.000000000000000000, 0.000000000000000000 ) ) ;
#6118 = CARTESIAN_POINT ( 'NONE',  ( 0.3106000600989253235, -3.122278952918442041, 4.592054218142292754 ) ) ;
#6119 = DIRECTION ( 'NONE',  ( 0.000000000000000000, 0.000000000000000000, -1.000000000000000000 ) ) ;
#6120 = ORIENTED_EDGE ( 'NONE', *, *, #5830, .F. ) ;
#6121 = AXIS2_PLACEMENT_3D ( 'NONE', #10754, #1899, #4190 ) ;
#6122 = FILL_AREA_STYLE_COLOUR ( '', #901 ) ;
#6123 = DIRECTION ( 'NONE',  ( -1.387778780781446464E-15, 2.775557561562892929E-15, 1.000000000000000000 ) ) ;
#6124 = ORIENTED_EDGE ( 'NONE', *, *, #6692, .F. ) ;
#6125 = CARTESIAN_POINT ( 'NONE',  ( 723.8855453127956707, 217.2873478855649694, -177.6000000000007617 ) ) ;
#6126 = ORIENTED_EDGE ( 'NONE', *, *, #14606, .F. ) ;
#6127 = DIRECTION ( 'NONE',  ( -0.9578262852211500977, 0.2873478855663498255, -1.110223024625158907E-15 ) ) ;
#6128 = EDGE_CURVE ( 'NONE', #3145, #6453, #4336, .T. ) ;
#6129 = EDGE_CURVE ( 'NONE', #11431, #1652, #6061, .T. ) ;
#6130 = CARTESIAN_POINT ( 'NONE',  ( 5.979512004945807924, -4.053280633787082365, -0.5609245978742287697 ) ) ;
#6132 = VECTOR ( 'NONE', #12094, 1000.000000000000000 ) ;
#6131 = CARTESIAN_POINT ( 'NONE',  ( 8.500000000000000000, 2.886751345948125547, 4.999999999999999112 ) ) ;
#6133 = EDGE_CURVE ( 'NONE', #12527, #556, #8091, .T. ) ;
#6134 = AXIS2_PLACEMENT_3D ( 'NONE', #10219, #12350, #10141 ) ;
#6135 = DIRECTION ( 'NONE',  ( 0.000000000000000000, 1.000000000000000000, 0.000000000000000000 ) ) ;
#6136 = AXIS2_PLACEMENT_3D ( 'NONE', #2904, #8578, #9976 ) ;
#6137 = CARTESIAN_POINT ( 'NONE',  ( 0.1739375980333739413, -5.301268757141563981, 0.8179331680533016291 ) ) ;
#6138 = ORIENTED_EDGE ( 'NONE', *, *, #8274, .F. ) ;
#6139 = DIRECTION ( 'NONE',  ( 0.000000000000000000, 0.000000000000000000, -1.000000000000000000 ) ) ;
#6140 = FACE_OUTER_BOUND ( 'NONE', #10952, .T. ) ;
#6141 = DIRECTION ( 'NONE',  ( 0.000000000000000000, 0.000000000000000000, 1.000000000000000000 ) ) ;
#6142 = AXIS2_PLACEMENT_3D ( 'NONE', #89, #2405, #2470 ) ;
#6143 = CARTESIAN_POINT ( 'NONE',  ( 6.420058897733091463, 2.891482565094592339, 5.008194711943422028 ) ) ;
#6144 = ORIENTED_EDGE ( 'NONE', *, *, #11237, .F. ) ;
#6145 = VERTEX_POINT ( 'NONE', #10164 ) ;
#6146 = DIRECTION ( 'NONE',  ( 0.000000000000000000, 1.224646799147353207E-16, 1.000000000000000000 ) ) ;
#6147 = DIRECTION ( 'NONE',  ( 0.000000000000000000, 1.000000000000000000, 0.000000000000000000 ) ) ;
#6148 = DIRECTION ( 'NONE',  ( 1.000000000000000000, 0.000000000000000000, 0.000000000000000000 ) ) ;
#6149 = CONICAL_SURFACE ( 'NONE', #8751, 4.000000000000000000, 0.8911886515913786111 ) ;
#6150 = VECTOR ( 'NONE', #13434, 999.9999999999998863 ) ;
#6151 = LINE ( 'NONE', #11823, #12695 ) ;
#6152 = AXIS2_PLACEMENT_3D ( 'NONE', #12409, #4612, #13679 ) ;
#6153 = VERTEX_POINT ( 'NONE', #251 ) ;
#6154 = STYLED_ITEM ( 'NONE', ( #11475 ), #1061 ) ;
#6155 = FACE_OUTER_BOUND ( 'NONE', #9889, .T. ) ;
#6156 = CARTESIAN_POINT ( 'NONE',  ( 6.420058897733093239, -2.891482565094601220, -5.008194711943422917 ) ) ;
#6157 = DIRECTION ( 'NONE',  ( -1.000000000000000000, 0.000000000000000000, 0.000000000000000000 ) ) ;
#6158 = CARTESIAN_POINT ( 'NONE',  ( -8.505790995055013681, 418.4210031920606525, 190.0000000000000000 ) ) ;
#6159 = PRODUCT_DEFINITION_CONTEXT ( 'detailed design', #10364, 'design' ) ;
#6160 = LINE ( 'NONE', #10662, #6305 ) ;
#6161 = CARTESIAN_POINT ( 'NONE',  ( -6.473970235329672780E-16, -4.862606272033106691, -3.745885042887442395 ) ) ;
#6162 = CIRCLE ( 'NONE', #7816, 2.500000000000000444 ) ;
#6163 = VERTEX_POINT ( 'NONE', #11412 ) ;
#6164 = AXIS2_PLACEMENT_3D ( 'NONE', #8143, #12650, #7195 ) ;
#6165 = CARTESIAN_POINT ( 'NONE',  ( 590.0000000000000000, 0.000000000000000000, -210.0000000000000000 ) ) ;
#6166 = ORIENTED_EDGE ( 'NONE', *, *, #13021, .T. ) ;
#6167 = ORIENTED_EDGE ( 'NONE', *, *, #5544, .F. ) ;
#6168 = LINE ( 'NONE', #9411, #5233 ) ;
#6169 = VECTOR ( 'NONE', #13268, 1000.000000000000114 ) ;
#6170 = STYLED_ITEM ( 'NONE', ( #11029 ), #8625 ) ;
#6171 = FACE_OUTER_BOUND ( 'NONE', #3215, .T. ) ;
#6172 = CIRCLE ( 'NONE', #11818, 7.500000000000062172 ) ;
#6173 = EDGE_CURVE ( 'NONE', #9769, #13350, #11473, .T. ) ;
#6174 = LINE ( 'NONE', #7345, #6290 ) ;
#6175 = FACE_OUTER_BOUND ( 'NONE', #6679, .T. ) ;
#6176 = EDGE_LOOP ( 'NONE', ( #14198, #10079, #13766, #9817 ) ) ;
#6177 = PLANE ( 'NONE',  #10417 ) ;
#6178 = FACE_OUTER_BOUND ( 'NONE', #5476, .T. ) ;
#6179 = CARTESIAN_POINT ( 'NONE',  ( 0.000000000000000000, 0.000000000000000000, -6.800000000000000711 ) ) ;
#6180 = CARTESIAN_POINT ( 'NONE',  ( 601.4378431141736883, -180.4313529342554432, 150.0000000000013358 ) ) ;
#6181 = EDGE_LOOP ( 'NONE', ( #13951, #4402, #6584, #13996 ) ) ;
#6182 = PRESENTATION_STYLE_ASSIGNMENT (( #9350 ) ) ;
#6183 = CARTESIAN_POINT ( 'NONE',  ( 6.403457969954074791, 2.888443235695460576, -5.002930439003194785 ) ) ;
#6184 = EDGE_LOOP ( 'NONE', ( #13945, #5804 ) ) ;
#6185 = AXIS2_PLACEMENT_3D ( 'NONE', #8982, #2473, #1365 ) ;
#6186 = FACE_BOUND ( 'NONE', #1229, .T. ) ;
#6187 = FACE_OUTER_BOUND ( 'NONE', #6962, .T. ) ;
#6188 = CARTESIAN_POINT ( 'NONE',  ( 0.000000000000000000, 0.000000000000000000, -4.000000000000000000 ) ) ;
#6189 = EDGE_CURVE ( 'NONE', #197, #14559, #12592, .T. ) ;
#6190 = DIRECTION ( 'NONE',  ( -0.000000000000000000, -0.000000000000000000, 1.000000000000000000 ) ) ;
#6191 = AXIS2_PLACEMENT_3D ( 'NONE', #3012, #14376, #11127 ) ;
#6192 = ORIENTED_EDGE ( 'NONE', *, *, #13640, .T. ) ;
#6193 = CARTESIAN_POINT ( 'NONE',  ( 610.0835668916889745, 190.4817695994259736, 186.9427398886703315 ) ) ;
#6194 = CARTESIAN_POINT ( 'NONE',  ( 610.4468987511024807, 188.9818594558784355, -185.9044171606945497 ) ) ;
#6195 = CARTESIAN_POINT ( 'NONE',  ( -0.5000000000000000000, -6.429618962271402616, 0.000000000000000000 ) ) ;
#6196 = DIRECTION ( 'NONE',  ( -1.387778780781446464E-15, 2.775557561562892929E-15, 1.000000000000000000 ) ) ;
#6197 = ORIENTED_EDGE ( 'NONE', *, *, #3635, .F. ) ;
#6198 = EDGE_CURVE ( 'NONE', #11788, #2298, #2278, .T. ) ;
#6199 = FACE_OUTER_BOUND ( 'NONE', #6508, .T. ) ;
#6200 = LINE ( 'NONE', #7074, #2521 ) ;
#6201 = VERTEX_POINT ( 'NONE', #4485 ) ;
#6202 = EDGE_CURVE ( 'NONE', #6883, #11959, #8747, .T. ) ;
#6203 = ORIENTED_EDGE ( 'NONE', *, *, #769, .T. ) ;
#6204 = CIRCLE ( 'NONE', #5960, 8.099999999999999645 ) ;
#6205 = CARTESIAN_POINT ( 'NONE',  ( 3.528928113779637776, -5.468125903023631551, -5.911160594572010107E-15 ) ) ;
#6206 = DIRECTION ( 'NONE',  ( 0.9578262852211513190, -0.2873478855663453846, 0.000000000000000000 ) ) ;
#6207 = CARTESIAN_POINT ( 'NONE',  ( -0.1481481481481481122, -4.797713218419819903, 0.000000000000000000 ) ) ;
#6208 = UNCERTAINTY_MEASURE_WITH_UNIT (LENGTH_MEASURE( 1.000000000000000082E-05 ), #1711, 'distance_accuracy_value', 'NONE');
#6209 = PLANE ( 'NONE',  #814 ) ;
#6210 = ORIENTED_EDGE ( 'NONE', *, *, #10243, .T. ) ;
#6211 = ADVANCED_FACE ( 'NONE', ( #8904, #6979, #7882 ), #5873, .F. ) ;
#6212 = CLOSED_SHELL ( 'NONE', ( #7208, #10728, #833, #6466, #13129, #7909, #8020, #2727, #11590, #364, #782, #3484, #6318, #13409, #8369, #4578, #6372, #10840, #785, #4497, #4305, #5948, #13511, #2005, #2885, #282, #13851, #9822, #11354, #11483, #12335, #6713 ) ) ;
#6213 = CARTESIAN_POINT ( 'NONE',  ( -10.00000000000000000, 10.00000000000000178, 190.0000000000000000 ) ) ;
#6214 = CARTESIAN_POINT ( 'NONE',  ( -31.74999999999995737, 0.000000000000000000, 0.000000000000000000 ) ) ;
#6215 = DIRECTION ( 'NONE',  ( 0.000000000000000000, 0.000000000000000000, 1.000000000000000000 ) ) ;
#6217 = EDGE_CURVE ( 'NONE', #10525, #151, #8370, .T. ) ;
#6216 = DIRECTION ( 'NONE',  ( 0.000000000000000000, 0.000000000000000000, 1.000000000000000000 ) ) ;
#6218 = ORIENTED_EDGE ( 'NONE', *, *, #12129, .T. ) ;
#6219 = EDGE_LOOP ( 'NONE', ( #9754, #3525, #13052, #5, #13074, #14244 ) ) ;
#6220 = PLANE ( 'NONE',  #14563 ) ;
#6221 = LINE ( 'NONE', #5052, #13917 ) ;
#6222 = CARTESIAN_POINT ( 'NONE',  ( 590.0000000000000000, 10.00000000000005507, -210.0000000000000000 ) ) ;
#6223 = CARTESIAN_POINT ( 'NONE',  ( -8.074769166705396017, 378.0965165842501392, 187.0000000000000284 ) ) ;
#6224 = ORIENTED_EDGE ( 'NONE', *, *, #5673, .T. ) ;
#6225 = DIRECTION ( 'NONE',  ( 1.000000000000000000, 0.000000000000000000, 0.000000000000000000 ) ) ;
#6226 = CARTESIAN_POINT ( 'NONE',  ( 0.000000000000000000, 8.572527594031473190E-16, -7.000000000000000000 ) ) ;
#6227 = CARTESIAN_POINT ( 'NONE',  ( 164.3243839102495656, 402.9042173714779551, 210.0000000000000000 ) ) ;
#6228 = CARTESIAN_POINT ( 'NONE',  ( 0.000000000000000000, 0.000000000000000000, -4.000000000000000000 ) ) ;
#6229 = DIRECTION ( 'NONE',  ( -0.2873478855663487708, -0.9578262852211504308, 3.876982066721826743E-15 ) ) ;
#6230 = CARTESIAN_POINT ( 'NONE',  ( 443.6584422793565636, 264.0194060144110608, -210.0000000000000000 ) ) ;
#6231 = ORIENTED_EDGE ( 'NONE', *, *, #9158, .F. ) ;
#6232 = CARTESIAN_POINT ( 'NONE',  ( 6.500000000000000000, 3.752776749732573247, -0.8000000000000003775 ) ) ;
#6233 = ORIENTED_EDGE ( 'NONE', *, *, #12631, .T. ) ;
#6234 = ORIENTED_EDGE ( 'NONE', *, *, #8635, .F. ) ;
#6235 = CARTESIAN_POINT ( 'NONE',  ( 451.6722694765949768, 316.6998517015743460, 190.0000000000000000 ) ) ;
#6236 = EDGE_CURVE ( 'NONE', #145, #10831, #9202, .T. ) ;
#6237 = PLANE ( 'NONE',  #6617 ) ;
#6238 = PLANE ( 'NONE',  #10536 ) ;
#6239 = EDGE_CURVE ( 'NONE', #8256, #3065, #5399, .T. ) ;
#6240 = CARTESIAN_POINT ( 'NONE',  ( 636.9746078850427011, 155.6249658629529620, -211.0000000000000000 ) ) ;
#6241 = ORIENTED_EDGE ( 'NONE', *, *, #6017, .F. ) ;
#6242 = DIRECTION ( 'NONE',  ( -0.000000000000000000, -0.000000000000000000, 1.000000000000000000 ) ) ;
#6243 = CARTESIAN_POINT ( 'NONE',  ( 642.5000000000001137, 160.0000000000000284, 210.0000059999999849 ) ) ;
#6244 = FACE_OUTER_BOUND ( 'NONE', #8366, .T. ) ;
#6245 = FACE_OUTER_BOUND ( 'NONE', #5568, .T. ) ;
#6246 =( NAMED_UNIT ( * ) SI_UNIT ( $, .STERADIAN. ) SOLID_ANGLE_UNIT ( ) );
#6247 = ORIENTED_EDGE ( 'NONE', *, *, #3933, .F. ) ;
#6248 = DIRECTION ( 'NONE',  ( 0.3543563944859323134, -0.9351104457158685435, 0.000000000000000000 ) ) ;
#6249 = ORIENTED_EDGE ( 'NONE', *, *, #1119, .T. ) ;
#6250 = ADVANCED_FACE ( 'NONE', ( #27 ), #3443, .F. ) ;
#6251 = DIRECTION ( 'NONE',  ( 0.9578262852211498757, -0.2873478855663502141, 1.489419751501264324E-15 ) ) ;
#6252 = FACE_OUTER_BOUND ( 'NONE', #3389, .T. ) ;
#6253 = CARTESIAN_POINT ( 'NONE',  ( -3.309651814758565180, -5.455921364805393026, -1.000000000000000000 ) ) ;
#6254 = EDGE_LOOP ( 'NONE', ( #3603, #4974, #6351 ) ) ;
#6255 = DIRECTION ( 'NONE',  ( 9.794481010665704304E-16, 3.264827003555233190E-15, 1.000000000000000000 ) ) ;
#6256 = FACE_BOUND ( 'NONE', #7681, .T. ) ;
#6257 = DIRECTION ( 'NONE',  ( -0.000000000000000000, -0.000000000000000000, -1.000000000000000000 ) ) ;
#6258 = CARTESIAN_POINT ( 'NONE',  ( 0.1750025118121568690, 4.719839900820621104, -3.469254087858248070 ) ) ;
#6259 = EDGE_LOOP ( 'NONE', ( #5079, #6766, #1519 ) ) ;
#6260 = CARTESIAN_POINT ( 'NONE',  ( 601.4378431141741430, -180.4313529342555569, -149.9999999999986642 ) ) ;
#6261 = DIRECTION ( 'NONE',  ( 1.000000000000000000, 0.000000000000000000, 0.000000000000000000 ) ) ;
#6262 = ORIENTED_EDGE ( 'NONE', *, *, #2696, .F. ) ;
#6263 = EDGE_CURVE ( 'NONE', #13510, #10292, #12437, .T. ) ;
#6264 = VERTEX_POINT ( 'NONE', #6838 ) ;
#6265 = DIRECTION ( 'NONE',  ( -1.000000000000000000, -0.000000000000000000, -0.000000000000000000 ) ) ;
#6266 = DIRECTION ( 'NONE',  ( 1.000000000000000000, 0.000000000000000000, 0.000000000000000000 ) ) ;
#6267 = CARTESIAN_POINT ( 'NONE',  ( -10.00000000000000000, 413.4403065089105667, 190.0000000000000000 ) ) ;
#6268 = LINE ( 'NONE', #4074, #12987 ) ;
#6269 = LINE ( 'NONE', #11940, #7895 ) ;
#6270 = EDGE_LOOP ( 'NONE', ( #255, #9779, #1774, #4210 ) ) ;
#6271 = CARTESIAN_POINT ( 'NONE',  ( 0.01055556052338940849, 4.575665857285979854, 2.074714256722482553 ) ) ;
#6272 = DIRECTION ( 'NONE',  ( 1.000000000000000000, 0.000000000000000000, 0.000000000000000000 ) ) ;
#6273 = DIRECTION ( 'NONE',  ( 0.000000000000000000, 0.000000000000000000, -1.000000000000000000 ) ) ;
#6274 = ADVANCED_FACE ( 'NONE', ( #11344 ), #13711, .F. ) ;
#6275 = EDGE_CURVE ( 'NONE', #7674, #10838, #4632, .T. ) ;
#6276 = PLANE ( 'NONE',  #4739 ) ;
#6277 = ORIENTED_EDGE ( 'NONE', *, *, #4185, .T. ) ;
#6278 = ORIENTED_EDGE ( 'NONE', *, *, #5893, .F. ) ;
#6279 = CARTESIAN_POINT ( 'NONE',  ( 636.7009106935324780, 155.5114698605638637, -210.0000000000000000 ) ) ;
#6280 = DIRECTION ( 'NONE',  ( 0.000000000000000000, 0.000000000000000000, 1.000000000000000000 ) ) ;
#6281 = EDGE_CURVE ( 'NONE', #5068, #13831, #5826, .T. ) ;
#6282 = DIRECTION ( 'NONE',  ( 0.000000000000000000, 0.000000000000000000, 1.000000000000000000 ) ) ;
#6283 = EDGE_CURVE ( 'NONE', #12986, #9079, #3746, .T. ) ;
#6284 = ADVANCED_FACE ( 'NONE', ( #9421 ), #3895, .F. ) ;
#6285 = DIRECTION ( 'NONE',  ( -0.000000000000000000, -0.000000000000000000, 1.000000000000000000 ) ) ;
#6286 = EDGE_LOOP ( 'NONE', ( #6007, #12364, #10716, #2737, #8643, #3 ) ) ;
#6287 = EDGE_CURVE ( 'NONE', #13316, #12842, #7135, .T. ) ;
#6288 = CARTESIAN_POINT ( 'NONE',  ( 1.600000000000000089, 0.000000000000000000, 0.000000000000000000 ) ) ;
#6289 = CARTESIAN_POINT ( 'NONE',  ( 0.3572655899081607078, 2.309401076758500704, -4.000000000000000000 ) ) ;
#6290 = VECTOR ( 'NONE', #685, 1000.000000000000000 ) ;
#6291 = FACE_OUTER_BOUND ( 'NONE', #6219, .T. ) ;
#6292 = CARTESIAN_POINT ( 'NONE',  ( 5.686050877451574337, -5.768780236673276995, -1.000000000000000000 ) ) ;
#6293 = FACE_OUTER_BOUND ( 'NONE', #7581, .T. ) ;
#6294 = FILL_AREA_STYLE_COLOUR ( '', #12532 ) ;
#6295 = PRODUCT_DEFINITION_SHAPE ( 'NONE', 'NONE',  #14634 ) ;
#6296 = ORIENTED_EDGE ( 'NONE', *, *, #373, .F. ) ;
#6297 = CARTESIAN_POINT ( 'NONE',  ( -6.259644161404860030E-16, -4.618802153517027165, -3.433295621305388234 ) ) ;
#6298 = EDGE_LOOP ( 'NONE', ( #14175, #3867, #1892, #5657 ) ) ;
#6299 = ORIENTED_EDGE ( 'NONE', *, *, #1225, .T. ) ;
#6300 = CARTESIAN_POINT ( 'NONE',  ( 227.7315295682384999, 303.4917135554678680, -177.6000000000009038 ) ) ;
#6301 = EDGE_CURVE ( 'NONE', #11494, #5554, #3713, .T. ) ;
#6302 = MECHANICAL_DESIGN_GEOMETRIC_PRESENTATION_REPRESENTATION (  '', ( #13365 ), #3010 ) ;
#6303 = EDGE_CURVE ( 'NONE', #2990, #12479, #12885, .T. ) ;
#6304 = CARTESIAN_POINT ( 'NONE',  ( 459.7035746174795463, 294.6698471414878782, -190.0000000000000000 ) ) ;
#6305 = VECTOR ( 'NONE', #304, 1000.000000000000114 ) ;
#6306 = LINE ( 'NONE', #10738, #12414 ) ;
#6307 = CARTESIAN_POINT ( 'NONE',  ( 590.0000000000000000, 0.000000000000000000, 190.0000000000000000 ) ) ;
#6308 = CIRCLE ( 'NONE', #14556, 5.525000000000000355 ) ;
#6309 = PRODUCT_DEFINITION_SHAPE ( 'NONE', 'NONE',  #5765 ) ;
#6310 = ORIENTED_EDGE ( 'NONE', *, *, #3556, .F. ) ;
#6311 = CARTESIAN_POINT ( 'NONE',  ( 6.507056315241511513, -2.833450876375909644, 5.092319121366348789 ) ) ;
#6312 =( REPRESENTATION_RELATIONSHIP ('NONE','NONE', #2822, #9337 ) REPRESENTATION_RELATIONSHIP_WITH_TRANSFORMATION ( #13802 )SHAPE_REPRESENTATION_RELATIONSHIP( ) );
#6313 = CARTESIAN_POINT ( 'NONE',  ( 641.5533979126568056, 163.7771423527817944, 210.0000119999999981 ) ) ;
#6314 = DIRECTION ( 'NONE',  ( 0.9578262852211513190, -0.2873478855663455511, 1.972152263052529951E-31 ) ) ;
#6315 = CARTESIAN_POINT ( 'NONE',  ( 229.2257385731838042, 308.4724102386206255, 177.5999999999999091 ) ) ;
#6316 =( NAMED_UNIT ( * ) SI_UNIT ( $, .STERADIAN. ) SOLID_ANGLE_UNIT ( ) );
#6317 = VERTEX_POINT ( 'NONE', #388 ) ;
#6318 = ADVANCED_FACE ( 'NONE', ( #12818 ), #553, .T. ) ;
#6319 = DIRECTION ( 'NONE',  ( -1.000000000000000000, -6.938893903907222067E-15, 0.000000000000000000 ) ) ;
#6320 = DIRECTION ( 'NONE',  ( -0.000000000000000000, -0.000000000000000000, -1.000000000000000000 ) ) ;
#6321 = ORIENTED_EDGE ( 'NONE', *, *, #1048, .F. ) ;
#6322 = ADVANCED_FACE ( 'NONE', ( #1670 ), #13782, .F. ) ;
#6323 = ORIENTED_EDGE ( 'NONE', *, *, #1046, .T. ) ;
#6324 = CARTESIAN_POINT ( 'NONE',  ( 1.400000000000000133, 0.000000000000000000, 0.000000000000000000 ) ) ;
#6325 = CARTESIAN_POINT ( 'NONE',  ( 446.3084422793565409, 264.0194060144110608, 190.0000000000000000 ) ) ;
#6326 = VECTOR ( 'NONE', #9747, 1000.000000000000114 ) ;
#6327 = VECTOR ( 'NONE', #5837, 1000.000000000000114 ) ;
#6328 = VECTOR ( 'NONE', #12276, 1000.000000000000000 ) ;
#6329 = ORIENTED_EDGE ( 'NONE', *, *, #12076, .F. ) ;
#6330 = CARTESIAN_POINT ( 'NONE',  ( 0.000000000000000000, 0.000000000000000000, 5.000000000000000888 ) ) ;
#6331 = CARTESIAN_POINT ( 'NONE',  ( 635.0000000000000000, 160.0000000000000284, -187.5000000000000000 ) ) ;
#6332 = CARTESIAN_POINT ( 'NONE',  ( 610.7992194312785159, 188.5714065965581483, -184.9452975700425554 ) ) ;
#6333 = FILL_AREA_STYLE_COLOUR ( '', #7810 ) ;
#6334 = ORIENTED_EDGE ( 'NONE', *, *, #10628, .F. ) ;
#6335 = PLANE ( 'NONE',  #12465 ) ;
#6336 =( NAMED_UNIT ( * ) PLANE_ANGLE_UNIT ( ) SI_UNIT ( $, .RADIAN. ) );
#6337 = VERTEX_POINT ( 'NONE', #1454 ) ;
#6338 = VECTOR ( 'NONE', #2709, 1000.000000000000227 ) ;
#6339 = TOROIDAL_SURFACE ( 'NONE', #2806, 2.700000000000000622, 0.2000000000000000111 ) ;
#6340 = VERTEX_POINT ( 'NONE', #4927 ) ;
#6341 = FACE_OUTER_BOUND ( 'NONE', #13786, .T. ) ;
#6342 = DIRECTION ( 'NONE',  ( 0.000000000000000000, -1.067522139062705339E-14, -1.000000000000000000 ) ) ;
#6343 = VECTOR ( 'NONE', #889, 1000.000000000000000 ) ;
#6344 = CARTESIAN_POINT ( 'NONE',  ( 6.204460410672268722, 3.831267809383453571, -3.364049496744554002 ) ) ;
#6345 = EDGE_CURVE ( 'NONE', #3667, #14024, #10303, .T. ) ;
#6346 = CARTESIAN_POINT ( 'NONE',  ( 139.8040310085880833, 355.9707293956415697, 210.0000000000000000 ) ) ;
#6347 = AXIS2_PLACEMENT_3D ( 'NONE', #5543, #3408, #4596 ) ;
#6348 = AXIS2_PLACEMENT_3D ( 'NONE', #13406, #12295, #4709 ) ;
#6349 = PRODUCT_DEFINITION_CONTEXT ( 'detailed design', #1983, 'design' ) ;
#6350 = CARTESIAN_POINT ( 'NONE',  ( 42.80949999999999278, 0.000000000000000000, 0.000000000000000000 ) ) ;
#6351 = ORIENTED_EDGE ( 'NONE', *, *, #935, .T. ) ;
#6352 = FACE_OUTER_BOUND ( 'NONE', #11498, .T. ) ;
#6353 = CYLINDRICAL_SURFACE ( 'NONE', #3518, 8.099999999999999645 ) ;
#6354 = APPLICATION_PROTOCOL_DEFINITION ( 'draft international standard', 'automotive_design', 1998, #1983 ) ;
#6355 = TOROIDAL_SURFACE ( 'NONE', #916, 5.100000000000000533, 0.1000000000000001582 ) ;
#6356 = CARTESIAN_POINT ( 'NONE',  ( 451.3035746174797396, 294.6698471414878782, 190.0000000000000000 ) ) ;
#6357 = VERTEX_POINT ( 'NONE', #7353 ) ;
#6358 = VERTEX_POINT ( 'NONE', #3670 ) ;
#6359 = CARTESIAN_POINT ( 'NONE',  ( 630.0000000000000000, 160.0000000000000284, 215.5000000000000000 ) ) ;
#6360 = DIRECTION ( 'NONE',  ( 1.000000000000000000, 0.000000000000000000, 0.000000000000000000 ) ) ;
#6361 = AXIS2_PLACEMENT_3D ( 'NONE', #11999, #2245, #7725 ) ;
#6362 = AXIS2_PLACEMENT_3D ( 'NONE', #10458, #5076, #478 ) ;
#6363 = CARTESIAN_POINT ( 'NONE',  ( 609.6836880993740806, 187.1145182921505921, -188.2379512264755874 ) ) ;
#6364 = AXIS2_PLACEMENT_3D ( 'NONE', #895, #6597, #763 ) ;
#6365 = EDGE_CURVE ( 'NONE', #6877, #1238, #6072, .T. ) ;
#6366 = CARTESIAN_POINT ( 'NONE',  ( 642.0000000000000000, 153.0000000000000284, -233.5000000000000000 ) ) ;
#6367 = AXIS2_PLACEMENT_3D ( 'NONE', #4468, #3369, #4622 ) ;
#6368 = ORIENTED_EDGE ( 'NONE', *, *, #13088, .T. ) ;
#6369 = FACE_OUTER_BOUND ( 'NONE', #10614, .T. ) ;
#6370 = CARTESIAN_POINT ( 'NONE',  ( -6.815830331203685866, -1.210827632163352847E-13, -6.171384342982610960 ) ) ;
#6371 = ORIENTED_EDGE ( 'NONE', *, *, #9772, .T. ) ;
#6372 = ADVANCED_FACE ( 'NONE', ( #9347 ), #14326, .T. ) ;
#6373 = AXIS2_PLACEMENT_3D ( 'NONE', #8882, #3279, #12195 ) ;
#6374 = DIRECTION ( 'NONE',  ( 0.000000000000000000, 0.000000000000000000, 1.000000000000000000 ) ) ;
#6375 = FACE_OUTER_BOUND ( 'NONE', #6687, .T. ) ;
#6376 = CARTESIAN_POINT ( 'NONE',  ( 142.4540310085880606, 355.9707293956415697, 190.0000000000000000 ) ) ;
#6377 = SURFACE_STYLE_FILL_AREA ( #9915 ) ;
#6378 = VERTEX_POINT ( 'NONE', #1522 ) ;
#6379 = ADVANCED_FACE ( 'NONE', ( #6244 ), #9033, .F. ) ;
#6380 = CARTESIAN_POINT ( 'NONE',  ( 0.2500000000000002220, 0.000000000000000000, 0.000000000000000000 ) ) ;
#6381 = ORIENTED_EDGE ( 'NONE', *, *, #5655, .F. ) ;
#6382 = VERTEX_POINT ( 'NONE', #14221 ) ;
#6383 = AXIS2_PLACEMENT_3D ( 'NONE', #11219, #3406, #7906 ) ;
#6384 = CARTESIAN_POINT ( 'NONE',  ( 1.567478505476134606E-15, 4.618802153517012066, -3.433295621305382905 ) ) ;
#6385 = AXIS2_PLACEMENT_3D ( 'NONE', #11519, #1339, #6059 ) ;
#6386 = ADVANCED_FACE ( 'NONE', ( #3149 ), #9642, .F. ) ;
#6387 = AXIS2_PLACEMENT_3D ( 'NONE', #1703, #7302, #6206 ) ;
#6388 = AXIS2_PLACEMENT_3D ( 'NONE', #1605, #2788, #2873 ) ;
#6389 = CARTESIAN_POINT ( 'NONE',  ( 1.600000000000000089, 0.000000000000000000, 0.000000000000000000 ) ) ;
#6390 = ORIENTED_EDGE ( 'NONE', *, *, #8135, .T. ) ;
#6391 = VECTOR ( 'NONE', #1620, 1000.000000000000000 ) ;
#6392 = EDGE_LOOP ( 'NONE', ( #13458, #11267, #234, #2283 ) ) ;
#6393 = CARTESIAN_POINT ( 'NONE',  ( 6.506891779418576327, -5.826362946429632927, -0.09155664655281940678 ) ) ;
#6394 = CARTESIAN_POINT ( 'NONE',  ( -9.999999999999998224, 376.8992337277234128, -187.0000000000000000 ) ) ;
#6395 = VECTOR ( 'NONE', #8973, 1000.000000000000000 ) ;
#6396 = CARTESIAN_POINT ( 'NONE',  ( 723.3240306373311341, 157.9460551874148564, 150.0000000000013642 ) ) ;
#6397 = DIRECTION ( 'NONE',  ( 0.2873478855663431086, 0.9578262852211520961, 1.261617073437853688E-14 ) ) ;
#6398 = ORIENTED_EDGE ( 'NONE', *, *, #2214, .T. ) ;
#6399 = EDGE_CURVE ( 'NONE', #8478, #6458, #10550, .T. ) ;
#6400 = AXIS2_PLACEMENT_3D ( 'NONE', #4479, #7662, #1140 ) ;
#6401 = EDGE_CURVE ( 'NONE', #4085, #8693, #5291, .T. ) ;
#6402 = PRESENTATION_LAYER_ASSIGNMENT (  '', '', ( #3088 ) ) ;
#6403 = CARTESIAN_POINT ( 'NONE',  ( 145.1678582058265192, 408.6511750828049117, -210.0000000000000000 ) ) ;
#6404 = CARTESIAN_POINT ( 'NONE',  ( 703.1581845006096501, 166.2926764603917036, -177.6000000000005059 ) ) ;
#6405 = ORIENTED_EDGE ( 'NONE', *, *, #2854, .F. ) ;
#6406 = CARTESIAN_POINT ( 'NONE',  ( 144.7991633467111683, 386.6211705227183870, -190.0000000000000000 ) ) ;
#6407 = EDGE_CURVE ( 'NONE', #13510, #13547, #5140, .T. ) ;
#6408 = VERTEX_POINT ( 'NONE', #10898 ) ;
#6409 = VECTOR ( 'NONE', #5023, 1000.000000000000000 ) ;
#6410 = AXIS2_PLACEMENT_3D ( 'NONE', #6675, #2292, #5707 ) ;
#6411 = DIRECTION ( 'NONE',  ( -0.000000000000000000, -0.000000000000000000, 1.000000000000000000 ) ) ;
#6412 = DIRECTION ( 'NONE',  ( -0.000000000000000000, -0.000000000000000000, 1.000000000000000000 ) ) ;
#6413 = VERTEX_POINT ( 'NONE', #909 ) ;
#6414 = CARTESIAN_POINT ( 'NONE',  ( 4.000000000000000000, -2.309401076758516691, -0.4999999999999995559 ) ) ;
#6415 = CARTESIAN_POINT ( 'NONE',  ( -1.500000000000000444, 5.750000000000000000, 0.000000000000000000 ) ) ;
#6416 = CARTESIAN_POINT ( 'NONE',  ( 635.0000000000000000, 160.0000000000000284, -210.0000000000000000 ) ) ;
#6417 = DIRECTION ( 'NONE',  ( 1.000000000000000000, 0.000000000000000000, 0.000000000000000000 ) ) ;
#6418 = AXIS2_PLACEMENT_3D ( 'NONE', #10741, #4172, #612 ) ;
#6419 = ORIENTED_EDGE ( 'NONE', *, *, #9471, .F. ) ;
#6420 = CARTESIAN_POINT ( 'NONE',  ( 6.534838248920897819, 2.951765777552412651, 5.112608298763836601 ) ) ;
#6421 = CARTESIAN_POINT ( 'NONE',  ( -6.500000000000000000, 3.149025070564754003, -0.5705737632551073357 ) ) ;
#6422 = ORIENTED_EDGE ( 'NONE', *, *, #11803, .T. ) ;
#6423 =( GEOMETRIC_REPRESENTATION_CONTEXT ( 3 ) GLOBAL_UNCERTAINTY_ASSIGNED_CONTEXT ( ( #7388 ) ) GLOBAL_UNIT_ASSIGNED_CONTEXT ( ( #3883, #1651, #10664 ) ) REPRESENTATION_CONTEXT ( 'NONE', 'WORKASPACE' ) );
#6424 = ORIENTED_EDGE ( 'NONE', *, *, #9772, .F. ) ;
#6425 = CARTESIAN_POINT ( 'NONE',  ( 610.8620436566991430, 188.5525593289319488, 184.8000000000000398 ) ) ;
#6426 = CARTESIAN_POINT ( 'NONE',  ( -1.891179505616666007E-13, -6.303931685388887194E-13, 189.9999999999986358 ) ) ;
#6427 = AXIS2_PLACEMENT_3D ( 'NONE', #10101, #13090, #1019 ) ;
#6428 = CARTESIAN_POINT ( 'NONE',  ( -9.137956343300963624, 416.3137853645741302, 190.0000000000000000 ) ) ;
#6429 = CARTESIAN_POINT ( 'NONE',  ( 642.0000000000000000, 167.0000000000000000, -233.5000000000000000 ) ) ;
#6430 = AXIS2_PLACEMENT_3D ( 'NONE', #8192, #2598, #7096 ) ;
#6431 = CARTESIAN_POINT ( 'NONE',  ( 635.0000000000000000, 160.0000000000000284, 210.0000119999999981 ) ) ;
#6432 = EDGE_CURVE ( 'NONE', #7052, #13396, #7952, .T. ) ;
#6433 = ORIENTED_EDGE ( 'NONE', *, *, #218, .F. ) ;
#6434 = PLANE ( 'NONE',  #12412 ) ;
#6435 = CARTESIAN_POINT ( 'NONE',  ( 590.0000000000000000, 212.5596934910894333, 210.0000000000000000 ) ) ;
#6436 = DIRECTION ( 'NONE',  ( 0.000000000000000000, 0.000000000000000000, -1.000000000000000000 ) ) ;
#6437 = AXIS2_PLACEMENT_3D ( 'NONE', #12152, #11045, #14240 ) ;
#6438 = DIRECTION ( 'NONE',  ( -1.000000000000000000, 0.000000000000000000, 0.000000000000000000 ) ) ;
#6439 = VERTEX_POINT ( 'NONE', #5353 ) ;
#6440 = VERTEX_POINT ( 'NONE', #9721 ) ;
#6441 = B_SPLINE_CURVE_WITH_KNOTS ( 'NONE', 3,
 ( #4636, #4490, #2418, #10238, #8094 ),
 .UNSPECIFIED., .F., .F.,
 ( 4, 1, 4 ),
 ( 0.000000000000000000, 0.002886751345948132021, 0.005773502691896264041 ),
 .UNSPECIFIED. ) ;
#6442 = CARTESIAN_POINT ( 'NONE',  ( -4.000000000000000000, 2.309401076758498483, -0.4999999999999927280 ) ) ;
#6443 = DIRECTION ( 'NONE',  ( 0.000000000000000000, 0.000000000000000000, 1.000000000000000000 ) ) ;
#6444 = ADVANCED_FACE ( 'NONE', ( #11027 ), #9934, .F. ) ;
#6445 = CIRCLE ( 'NONE', #6618, 5.199999999999760369 ) ;
#6446 = EDGE_CURVE ( 'NONE', #10292, #1912, #13321, .T. ) ;
#6447 = DIRECTION ( 'NONE',  ( -0.000000000000000000, -0.000000000000000000, 1.000000000000000000 ) ) ;
#6448 = COLOUR_RGB ( '',1.000000000000000000, 0.9490196078431372140, 0.9098039215686274384 ) ;
#6449 = LINE ( 'NONE', #10940, #8026 ) ;
#6450 = ORIENTED_EDGE ( 'NONE', *, *, #4681, .T. ) ;
#6451 = CIRCLE ( 'NONE', #1015, 5.100000000000000533 ) ;
#6452 = FACE_OUTER_BOUND ( 'NONE', #2186, .T. ) ;
#6453 = VERTEX_POINT ( 'NONE', #14360 ) ;
#6454 = B_SPLINE_CURVE_WITH_KNOTS ( 'NONE', 3,
 ( #63, #4529, #9023, #1188 ),
 .UNSPECIFIED., .F., .F.,
 ( 4, 4 ),
 ( 0.002977824986803846545, 0.005972417098209359745 ),
 .UNSPECIFIED. ) ;
#6455 = DIRECTION ( 'NONE',  ( 1.019665600948283447E-15, 3.398885336494278419E-15, -1.000000000000000000 ) ) ;
#6456 = DIRECTION ( 'NONE',  ( 0.000000000000000000, 0.000000000000000000, -1.000000000000000000 ) ) ;
#6457 = CARTESIAN_POINT ( 'NONE',  ( 707.5067158355136598, 162.6912496279593938, -177.6000000000005059 ) ) ;
#6458 = VERTEX_POINT ( 'NONE', #2090 ) ;
#6459 = DIRECTION ( 'NONE',  ( 0.9578262852211513190, -0.2873478855663454401, 0.000000000000000000 ) ) ;
#6460 = VERTEX_POINT ( 'NONE', #1803 ) ;
#6461 = ORIENTED_EDGE ( 'NONE', *, *, #9334, .F. ) ;
#6462 = DIRECTION ( 'NONE',  ( -0.9237280213470676626, -0.3830490080632388272, 0.000000000000000000 ) ) ;
#6463 = EDGE_CURVE ( 'NONE', #12209, #9351, #13107, .T. ) ;
#6464 = CARTESIAN_POINT ( 'NONE',  ( 707.5067158355135462, 162.6912496279604170, -177.6000000000005059 ) ) ;
#6466 = ADVANCED_FACE ( 'NONE', ( #692 ), #395, .T. ) ;
#6465 = ORIENTED_EDGE ( 'NONE', *, *, #8542, .F. ) ;
#6467 = ORIENTED_EDGE ( 'NONE', *, *, #8265, .T. ) ;
#6468 = DIRECTION ( 'NONE',  ( 1.000000000000000000, 0.000000000000000000, 0.000000000000000000 ) ) ;
#6469 = CARTESIAN_POINT ( 'NONE',  ( 627.6952049249875927, 161.9631091326946830, 210.0000119999999981 ) ) ;
#6470 = DIRECTION ( 'NONE',  ( -1.000000000000000000, 0.000000000000000000, 0.000000000000000000 ) ) ;
#6471 = DIRECTION ( 'NONE',  ( 0.000000000000000000, 0.000000000000000000, -1.000000000000000000 ) ) ;
#6472 = FILL_AREA_STYLE ('',( #4254 ) ) ;
#6473 = EDGE_LOOP ( 'NONE', ( #11598, #3054, #2026 ) ) ;
#6474 = CARTESIAN_POINT ( 'NONE',  ( 635.0000000000000000, 160.0000000000000284, -222.5000000000000000 ) ) ;
#6475 = ITEM_DEFINED_TRANSFORMATION ( 'NONE', 'NONE', #1228,  #9440 ) ;
#6476 = ORIENTED_EDGE ( 'NONE', *, *, #7002, .T. ) ;
#6477 = CARTESIAN_POINT ( 'NONE',  ( 0.000000000000000000, 0.000000000000000000, 0.000000000000000000 ) ) ;
#6478 = ADVANCED_FACE ( 'NONE', ( #8757 ), #14443, .F. ) ;
#6479 = ORIENTED_EDGE ( 'NONE', *, *, #5828, .F. ) ;
#6480 = CARTESIAN_POINT ( 'NONE',  ( 0.4465819873849480870, -2.886751345948518566, -5.000000000000000000 ) ) ;
#6481 = EDGE_CURVE ( 'NONE', #11836, #2452, #5432, .T. ) ;
#6482 = CARTESIAN_POINT ( 'NONE',  ( 0.000000000000000000, 0.000000000000000000, 5.000000000000000888 ) ) ;
#6483 = EDGE_CURVE ( 'NONE', #248, #14449, #2778, .T. ) ;
#6484 = ORIENTED_EDGE ( 'NONE', *, *, #1193, .F. ) ;
#6485 = CARTESIAN_POINT ( 'NONE',  ( 0.000000000000000000, 5.773502691896261751, -2.749426538070115714E-16 ) ) ;
#6486 = DIRECTION ( 'NONE',  ( -0.000000000000000000, -0.000000000000000000, 1.000000000000000000 ) ) ;
#6487 = ADVANCED_FACE ( 'NONE', ( #7712 ), #13618, .F. ) ;
#6488 = LINE ( 'NONE', #10977, #12550 ) ;
#6489 =( LENGTH_UNIT ( ) NAMED_UNIT ( * ) SI_UNIT ( .MILLI., .METRE. ) );
#6490 = EDGE_LOOP ( 'NONE', ( #840, #11714, #13876, #3677 ) ) ;
#6491 = DIRECTION ( 'NONE',  ( -0.2873478855663461062, -0.9578262852211510969, 6.938893903907199190E-15 ) ) ;
#6492 = ORIENTED_EDGE ( 'NONE', *, *, #7165, .F. ) ;
#6493 = VERTEX_POINT ( 'NONE', #11987 ) ;
#6494 = LINE ( 'NONE', #5525, #5857 ) ;
#6495 = DIRECTION ( 'NONE',  ( 0.9578262852211513190, -0.2873478855663453846, 0.000000000000000000 ) ) ;
#6496 = CARTESIAN_POINT ( 'NONE',  ( 2.999999999999999112, 0.000000000000000000, 0.000000000000000000 ) ) ;
#6497 = DIRECTION ( 'NONE',  ( -0.000000000000000000, -0.000000000000000000, 1.000000000000000000 ) ) ;
#6498 = UNCERTAINTY_MEASURE_WITH_UNIT (LENGTH_MEASURE( 1.000000000000000082E-05 ), #6489, 'distance_accuracy_value', 'NONE');
#6499 = CARTESIAN_POINT ( 'NONE',  ( -6.837824896291515131, -3.947820044545435447, -6.564402953523717166 ) ) ;
#6500 = ORIENTED_EDGE ( 'NONE', *, *, #3576, .F. ) ;
#6501 = ADVANCED_FACE ( 'NONE', ( #11912 ), #1883, .F. ) ;
#6502 = DIRECTION ( 'NONE',  ( 0.9578262852211515410, -0.2873478855663448850, -2.182720603638867417E-30 ) ) ;
#6503 = CARTESIAN_POINT ( 'NONE',  ( 6.244004651191002786, -4.663678638742300819, -2.132808149174402423 ) ) ;
#6504 = CARTESIAN_POINT ( 'NONE',  ( 446.3084422793564841, 264.0194060144110608, -183.5000000000000000 ) ) ;
#6505 = LINE ( 'NONE', #874, #12502 ) ;
#6506 = EDGE_CURVE ( 'NONE', #10347, #2358, #6685, .T. ) ;
#6507 = ORIENTED_EDGE ( 'NONE', *, *, #13862, .T. ) ;
#6508 = EDGE_LOOP ( 'NONE', ( #14266, #13697, #10010, #332, #1417 ) ) ;
#6509 = FACE_OUTER_BOUND ( 'NONE', #5475, .T. ) ;
#6510 = CARTESIAN_POINT ( 'NONE',  ( 636.9746078850427011, 155.6249658629529620, 211.0000000000000000 ) ) ;
#6511 = EDGE_CURVE ( 'NONE', #5031, #11833, #13387, .T. ) ;
#6512 = CARTESIAN_POINT ( 'NONE',  ( 609.9372209285376130, 185.6979141947072378, -185.1431837845556743 ) ) ;
#6513 = ADVANCED_BREP_SHAPE_REPRESENTATION ( '', ( #2557, #9440 ), #9925 ) ;
#6514 = DIRECTION ( 'NONE',  ( 0.000000000000000000, 0.000000000000000000, 1.000000000000000000 ) ) ;
#6515 = EDGE_LOOP ( 'NONE', ( #2478, #6465 ) ) ;
#6516 = DIRECTION ( 'NONE',  ( 0.000000000000000000, 0.000000000000000000, -1.000000000000000000 ) ) ;
#6517 = ORIENTED_EDGE ( 'NONE', *, *, #12519, .F. ) ;
#6518 = CARTESIAN_POINT ( 'NONE',  ( 610.0000000000000000, -9.999999999999941380, 210.0000000000000000 ) ) ;
#6519 = DIRECTION ( 'NONE',  ( 0.9578262852211503198, -0.2873478855663487153, 0.000000000000000000 ) ) ;
#6520 = LINE ( 'NONE', #13161, #13873 ) ;
#6521 = ORIENTED_EDGE ( 'NONE', *, *, #7837, .F. ) ;
#6522 = DIRECTION ( 'NONE',  ( -0.2873478855663454956, -0.9578262852211514300, 3.467246277775659127E-15 ) ) ;
#6523 = EDGE_LOOP ( 'NONE', ( #13139, #4880, #4399, #4707 ) ) ;
#6524 = EDGE_LOOP ( 'NONE', ( #640, #5097 ) ) ;
#6525 = CARTESIAN_POINT ( 'NONE',  ( 0.4465819873851997746, 2.886751345948125547, 4.999999999999999112 ) ) ;
#6526 = DIRECTION ( 'NONE',  ( 0.000000000000000000, 0.000000000000000000, -1.000000000000000000 ) ) ;
#6527 = CARTESIAN_POINT ( 'NONE',  ( -2.171643655288372443, 3.365003104552320767, 2.541098841762897165E-18 ) ) ;
#6528 = ORIENTED_EDGE ( 'NONE', *, *, #13871, .T. ) ;
#6529 = ORIENTED_EDGE ( 'NONE', *, *, #12956, .T. ) ;
#6530 = CARTESIAN_POINT ( 'NONE',  ( 6.323279575526099983, -3.325091652216674909, 4.240772318537645802 ) ) ;
#6531 = EDGE_CURVE ( 'NONE', #238, #11405, #8074, .T. ) ;
#6532 = CARTESIAN_POINT ( 'NONE',  ( 6.500000000000000888, 2.679956093905413450, -6.238387772031967593 ) ) ;
#6533 = CARTESIAN_POINT ( 'NONE',  ( 630.0000000000000000, 160.0000000000000284, 215.5000000000000000 ) ) ;
#6534 = CARTESIAN_POINT ( 'NONE',  ( -9.137956343300945861, 374.5525593289318635, 184.8000000000000114 ) ) ;
#6535 = CYLINDRICAL_SURFACE ( 'NONE', #5268, 2.649999999999985700 ) ;
#6536 = VERTEX_POINT ( 'NONE', #9182 ) ;
#6537 = CARTESIAN_POINT ( 'NONE',  ( 635.0000000000000000, 160.0000000000000284, -210.0000000000000000 ) ) ;
#6538 = ADVANCED_BREP_SHAPE_REPRESENTATION ( '', ( #2617, #9440 ), #1445 ) ;
#6539 = ORIENTED_EDGE ( 'NONE', *, *, #5091, .F. ) ;
#6540 = CARTESIAN_POINT ( 'NONE',  ( 0.000000000000000000, 0.000000000000000000, 0.000000000000000000 ) ) ;
#6541 = CONICAL_SURFACE ( 'NONE', #13874, 2.055000000000000160, 0.7853981633974639331 ) ;
#6542 = ORIENTED_EDGE ( 'NONE', *, *, #1119, .F. ) ;
#6543 = AXIS2_PLACEMENT_3D ( 'NONE', #10673, #3890, #546 ) ;
#6544 = FACE_OUTER_BOUND ( 'NONE', #3184, .T. ) ;
#6545 = CARTESIAN_POINT ( 'NONE',  ( 228.5935732249376429, 306.3651924111320568, -177.6000000000005059 ) ) ;
#6546 = EDGE_LOOP ( 'NONE', ( #7571, #7373, #1685, #3913 ) ) ;
#6547 = DIRECTION ( 'NONE',  ( 0.000000000000000000, -1.000000000000000000, 0.000000000000000000 ) ) ;
#6548 = ADVANCED_FACE ( 'NONE', ( #8884, #13688 ), #3500, .T. ) ;
#6549 = CARTESIAN_POINT ( 'NONE',  ( -9.511508594537115613, 378.5275384125997107, 190.0000000000000000 ) ) ;
#6550 = CIRCLE ( 'NONE', #3237, 0.7500000000000000000 ) ;
#6551 = VECTOR ( 'NONE', #13259, 1000.000000000000114 ) ;
#6552 = DIRECTION ( 'NONE',  ( 0.000000000000000000, 0.000000000000000000, 1.000000000000000000 ) ) ;
#6553 = EDGE_LOOP ( 'NONE', ( #3610, #11927, #1136, #6278 ) ) ;
#6554 = EDGE_CURVE ( 'NONE', #8892, #9095, #3283, .T. ) ;
#6555 = LINE ( 'NONE', #8842, #7988 ) ;
#6556 = VERTEX_POINT ( 'NONE', #79 ) ;
#6557 = EDGE_CURVE ( 'NONE', #2108, #11431, #5719, .T. ) ;
#6558 = ORIENTED_EDGE ( 'NONE', *, *, #12519, .T. ) ;
#6559 = CARTESIAN_POINT ( 'NONE',  ( 2.241046694638796133, -6.576374040525796438, -6.171384342982452864 ) ) ;
#6560 = AXIS2_PLACEMENT_3D ( 'NONE', #6940, #1545, #6868 ) ;
#6561 = ADVANCED_FACE ( 'NONE', ( #990 ), #9105, .F. ) ;
#6563 = VECTOR ( 'NONE', #14122, 1000.000000000000000 ) ;
#6562 = PLANE ( 'NONE',  #4461 ) ;
#6564 = CYLINDRICAL_SURFACE ( 'NONE', #1674, 5.000000000000000000 ) ;
#6565 = DIRECTION ( 'NONE',  ( -0.000000000000000000, -0.000000000000000000, -1.000000000000000000 ) ) ;
#6566 = CYLINDRICAL_SURFACE ( 'NONE', #8538, 5.200000000000009948 ) ;
#6567 = CYLINDRICAL_SURFACE ( 'NONE', #4841, 7.500000000000062172 ) ;
#6568 = ORIENTED_EDGE ( 'NONE', *, *, #3707, .T. ) ;
#6569 = AXIS2_PLACEMENT_3D ( 'NONE', #11716, #12912, #13128 ) ;
#6570 = AXIS2_PLACEMENT_3D ( 'NONE', #2733, #7094, #5045 ) ;
#6571 = FACE_OUTER_BOUND ( 'NONE', #1460, .T. ) ;
#6572 = CARTESIAN_POINT ( 'NONE',  ( -31.74999999999995737, 0.000000000000000000, 0.000000000000000000 ) ) ;
#6573 = EDGE_CURVE ( 'NONE', #13114, #6358, #13145, .T. ) ;
#6574 = ADVANCED_FACE ( 'NONE', ( #12497 ), #2303, .F. ) ;
#6575 = CARTESIAN_POINT ( 'NONE',  ( 635.0000000000000000, 160.0000000000000284, -187.5000000000000000 ) ) ;
#6576 = EDGE_LOOP ( 'NONE', ( #3218, #11514 ) ) ;
#6577 = ORIENTED_EDGE ( 'NONE', *, *, #8485, .T. ) ;
#6578 = DIRECTION ( 'NONE',  ( -0.9578262852211514300, 0.2873478855663453846, 9.382948195091500646E-16 ) ) ;
#6579 = EDGE_CURVE ( 'NONE', #2446, #3145, #968, .T. ) ;
#6580 = CARTESIAN_POINT ( 'NONE',  ( 101.4713065522755215, 338.2376885075850623, -1.342499394901007523E-12 ) ) ;
#6581 = AXIS2_PLACEMENT_3D ( 'NONE', #12188, #14495, #6676 ) ;
#6582 = VECTOR ( 'NONE', #12101, 1000.000000000000114 ) ;
#6583 = DIRECTION ( 'NONE',  ( -1.000000000000000000, -0.000000000000000000, -0.000000000000000000 ) ) ;
#6584 = ORIENTED_EDGE ( 'NONE', *, *, #12332, .T. ) ;
#6585 = CARTESIAN_POINT ( 'NONE',  ( -6.500000000000000888, -4.077972562205394169, -6.122137109124704324 ) ) ;
#6586 = EDGE_LOOP ( 'NONE', ( #6500, #14210 ) ) ;
#6587 = PRESENTATION_LAYER_ASSIGNMENT (  '', '', ( #11527 ) ) ;
#6588 = PLANE ( 'NONE',  #5846 ) ;
#6589 = PLANE ( 'NONE',  #11047 ) ;
#6590 = DIRECTION ( 'NONE',  ( 1.000000000000000000, 0.000000000000000000, 0.000000000000000000 ) ) ;
#6591 =( NAMED_UNIT ( * ) PLANE_ANGLE_UNIT ( ) SI_UNIT ( $, .RADIAN. ) );
#6592 = AXIS2_PLACEMENT_3D ( 'NONE', #6580, #6791, #11154 ) ;
#6593 = DIRECTION ( 'NONE',  ( 0.9578262852211507639, -0.2873478855663477716, 0.000000000000000000 ) ) ;
#6594 = CIRCLE ( 'NONE', #203, 2.499999999999946709 ) ;
#6595 = ORIENTED_EDGE ( 'NONE', *, *, #1459, .F. ) ;
#6596 = ORIENTED_EDGE ( 'NONE', *, *, #5034, .T. ) ;
#6597 = DIRECTION ( 'NONE',  ( 1.000000000000000000, 0.000000000000000000, 0.000000000000000000 ) ) ;
#6598 =( REPRESENTATION_RELATIONSHIP ('NONE','NONE', #2822, #5933 ) REPRESENTATION_RELATIONSHIP_WITH_TRANSFORMATION ( #12891 )SHAPE_REPRESENTATION_RELATIONSHIP( ) );
#6599 = DIRECTION ( 'NONE',  ( 0.000000000000000000, 0.000000000000000000, 1.000000000000000000 ) ) ;
#6600 = CIRCLE ( 'NONE', #926, 6.500000000000000888 ) ;
#6601 = DIRECTION ( 'NONE',  ( 1.000000000000000000, 0.000000000000000000, 0.000000000000000000 ) ) ;
#6602 = CIRCLE ( 'NONE', #6829, 6.500000000000000888 ) ;
#6603 = ORIENTED_EDGE ( 'NONE', *, *, #1243, .T. ) ;
#6604 = ORIENTED_EDGE ( 'NONE', *, *, #357, .F. ) ;
#6605 = CARTESIAN_POINT ( 'NONE',  ( 2.690931834596283156, -5.951943280390046276, -5.793705359219412742E-15 ) ) ;
#6606 = CARTESIAN_POINT ( 'NONE',  ( 610.0000000000000000, 227.4403065089105951, -210.0000000000000000 ) ) ;
#6607 = PLANE ( 'NONE',  #12687 ) ;
#6608 = DIRECTION ( 'NONE',  ( 1.000000000000000000, 0.000000000000000000, 0.000000000000000000 ) ) ;
#6609 = FACE_BOUND ( 'NONE', #12156, .T. ) ;
#6610 = VECTOR ( 'NONE', #5823, 1000.000000000000000 ) ;
#6611 = VERTEX_POINT ( 'NONE', #2172 ) ;
#6612 = AXIS2_PLACEMENT_3D ( 'NONE', #14475, #1094, #6865 ) ;
#6613 = CARTESIAN_POINT ( 'NONE',  ( 609.9641659369621038, 190.7604956903689413, 190.0000000000000568 ) ) ;
#6614 = CONTEXT_DEPENDENT_SHAPE_REPRESENTATION ( #4918, #6907 ) ;
#6615 = ORIENTED_EDGE ( 'NONE', *, *, #10660, .F. ) ;
#6616 = DIRECTION ( 'NONE',  ( 0.000000000000000000, 1.000000000000000000, 0.000000000000000000 ) ) ;
#6617 = AXIS2_PLACEMENT_3D ( 'NONE', #10737, #608, #7266 ) ;
#6618 = AXIS2_PLACEMENT_3D ( 'NONE', #8852, #4360, #2202 ) ;
#6619 = EDGE_LOOP ( 'NONE', ( #13805, #8843, #12462 ) ) ;
#6620 = EDGE_CURVE ( 'NONE', #13306, #11617, #5785, .T. ) ;
#6621 = EDGE_CURVE ( 'NONE', #5056, #11949, #8196, .T. ) ;
#6622 = LINE ( 'NONE', #13400, #12969 ) ;
#6623 = CIRCLE ( 'NONE', #3811, 6.975000000000000533 ) ;
#6624 = AXIS2_PLACEMENT_3D ( 'NONE', #275, #1480, #4814 ) ;
#6625 = DIRECTION ( 'NONE',  ( 0.03086419753086420623, -0.9995235871707959241, 0.000000000000000000 ) ) ;
#6626 = ORIENTED_EDGE ( 'NONE', *, *, #8640, .T. ) ;
#6627 = LINE ( 'NONE', #12002, #12047 ) ;
#6628 = CYLINDRICAL_SURFACE ( 'NONE', #10117, 2.199999999999730171 ) ;
#6629 = AXIS2_PLACEMENT_3D ( 'NONE', #14388, #10099, #12447 ) ;
#6630 = DIRECTION ( 'NONE',  ( -0.000000000000000000, -0.000000000000000000, 1.000000000000000000 ) ) ;
#6631 = ORIENTED_EDGE ( 'NONE', *, *, #8894, .T. ) ;
#6632 = ORIENTED_EDGE ( 'NONE', *, *, #8562, .F. ) ;
#6633 = AXIS2_PLACEMENT_3D ( 'NONE', #14162, #11862, #2871 ) ;
#6634 = CIRCLE ( 'NONE', #246, 0.7499999999999997780 ) ;
#6635 = ORIENTED_EDGE ( 'NONE', *, *, #10216, .F. ) ;
#6636 = CARTESIAN_POINT ( 'NONE',  ( 1.567478505476134606E-15, 4.618802153517012066, -5.000000000000000000 ) ) ;
#6637 = PRODUCT_DEFINITION_SHAPE ( 'NONE', 'NONE',  #972 ) ;
#6638 = ADVANCED_FACE ( 'NONE', ( #3366 ), #14570, .F. ) ;
#6639 = VECTOR ( 'NONE', #3006, 1000.000000000000114 ) ;
#6640 = STYLED_ITEM ( 'NONE', ( #2752 ), #7736 ) ;
#6641 = LINE ( 'NONE', #5378, #3778 ) ;
#6642 = CARTESIAN_POINT ( 'NONE',  ( 6.499999999999999112, -3.752776749732576356, -0.8000000000000003775 ) ) ;
#6643 = AXIS2_PLACEMENT_3D ( 'NONE', #13841, #9501, #11690 ) ;
#6644 = CARTESIAN_POINT ( 'NONE',  ( 707.5067158355137735, 173.1315561368707847, -149.9999999999986642 ) ) ;
#6645 = EDGE_CURVE ( 'NONE', #7999, #11993, #1126, .T. ) ;
#6646 = CARTESIAN_POINT ( 'NONE',  ( 3.999999999999999112, 1.941961291383486277, -0.3515519931180248192 ) ) ;
#6647 = DIRECTION ( 'NONE',  ( -1.000000000000000000, 0.000000000000000000, 0.000000000000000000 ) ) ;
#6648 = CARTESIAN_POINT ( 'NONE',  ( 0.3572655899081652042, 4.618802153517012066, 5.829523438926728986E-16 ) ) ;
#6649 = ORIENTED_EDGE ( 'NONE', *, *, #4134, .T. ) ;
#6650 = DIRECTION ( 'NONE',  ( 0.000000000000000000, 0.000000000000000000, -1.000000000000000000 ) ) ;
#6651 = LINE ( 'NONE', #12318, #11284 ) ;
#6652 = SHAPE_DEFINITION_REPRESENTATION ( #8658, #5290 ) ;
#6653 = DIRECTION ( 'NONE',  ( 0.000000000000000000, 0.000000000000000000, 1.000000000000000000 ) ) ;
#6654 = ORIENTED_EDGE ( 'NONE', *, *, #6128, .T. ) ;
#6655 = ORIENTED_EDGE ( 'NONE', *, *, #9384, .T. ) ;
#6656 = AXIS2_PLACEMENT_3D ( 'NONE', #13990, #2459, #6963 ) ;
#6657 = CARTESIAN_POINT ( 'NONE',  ( 705.2654023280957745, 165.6605111121449738, 150.0000000000013358 ) ) ;
#6658 = CARTESIAN_POINT ( 'NONE',  ( 6.367873360227558344, 5.773502691896261751, 0.000000000000000000 ) ) ;
#6659 = ADVANCED_FACE ( 'NONE', ( #11 ), #4548, .F. ) ;
#6660 = DIRECTION ( 'NONE',  ( -0.000000000000000000, -1.000000000000000000, -0.000000000000000000 ) ) ;
#6661 = PRODUCT_DEFINITION_FORMATION_WITH_SPECIFIED_SOURCE ( 'ANY', '', #124, .NOT_KNOWN. ) ;
#6662 = CARTESIAN_POINT ( 'NONE',  ( -9.137956343300997375, 374.5525593289318635, -169.9999999999999716 ) ) ;
#6663 = ORIENTED_EDGE ( 'NONE', *, *, #12675, .F. ) ;
#6664 = ADVANCED_FACE ( 'NONE', ( #13829 ), #2690, .F. ) ;
#6665 = UNCERTAINTY_MEASURE_WITH_UNIT (LENGTH_MEASURE( 1.000000000000000082E-05 ), #8676, 'distance_accuracy_value', 'NONE');
#6666 = CIRCLE ( 'NONE', #8547, 0.7499999999999997780 ) ;
#6667 = CARTESIAN_POINT ( 'NONE',  ( 635.0000000000000000, 160.0000000000000284, 187.5000000000000000 ) ) ;
#6668 = ORIENTED_EDGE ( 'NONE', *, *, #9191, .F. ) ;
#6669 = EDGE_CURVE ( 'NONE', #6036, #4450, #3721, .T. ) ;
#6670 = DIRECTION ( 'NONE',  ( 1.000000000000000000, 0.000000000000000000, 0.000000000000000000 ) ) ;
#6671 = DIRECTION ( 'NONE',  ( 9.794481010665704304E-16, 3.264827003555234768E-15, -1.000000000000000000 ) ) ;
#6672 = CARTESIAN_POINT ( 'NONE',  ( -2.100000000000000089, 2.571758278209441957E-16, -5.000000000000000000 ) ) ;
#6673 = EDGE_LOOP ( 'NONE', ( #3868, #4656, #3507, #11748 ) ) ;
#6674 = ORIENTED_EDGE ( 'NONE', *, *, #3645, .F. ) ;
#6675 = CARTESIAN_POINT ( 'NONE',  ( 635.0000000000000000, 160.0000000000000284, -190.0000000000000000 ) ) ;
#6676 = DIRECTION ( 'NONE',  ( 0.000000000000000000, 0.000000000000000000, 1.000000000000000000 ) ) ;
#6677 = AXIS2_PLACEMENT_3D ( 'NONE', #6288, #6225, #1785 ) ;
#6678 = DIRECTION ( 'NONE',  ( 1.000000000000000000, 0.000000000000000000, 0.000000000000000000 ) ) ;
#6679 = EDGE_LOOP ( 'NONE', ( #5819, #1427, #9988, #1263 ) ) ;
#6680 = EDGE_LOOP ( 'NONE', ( #6329, #10354, #11924, #11247 ) ) ;
#6681 = CARTESIAN_POINT ( 'NONE',  ( 610.0000000000001137, 191.1080398579019288, -190.0300000000000296 ) ) ;
#6682 = FACE_OUTER_BOUND ( 'NONE', #5312, .T. ) ;
#6683 = PRODUCT_RELATED_PRODUCT_CATEGORY ( 'part', '', ( #14090 ) ) ;
#6684 = CARTESIAN_POINT ( 'NONE',  ( -2.725741868435985094, 3.045094352034055429, -3.220599429844047012 ) ) ;
#6685 = LINE ( 'NONE', #10001, #4192 ) ;
#6686 = DIRECTION ( 'NONE',  ( 1.000000000000000000, 0.000000000000000000, 0.000000000000000000 ) ) ;
#6687 = EDGE_LOOP ( 'NONE', ( #4564, #5175, #10919, #9794 ) ) ;
#6688 = DIRECTION ( 'NONE',  ( -1.000000000000000000, -0.000000000000000000, -0.000000000000000000 ) ) ;
#6689 = ORIENTED_EDGE ( 'NONE', *, *, #2028, .F. ) ;
#6690 = ORIENTED_EDGE ( 'NONE', *, *, #7862, .T. ) ;
#6691 = PLANE ( 'NONE',  #10393 ) ;
#6692 = EDGE_CURVE ( 'NONE', #9303, #14092, #9487, .T. ) ;
#6693 = ORIENTED_EDGE ( 'NONE', *, *, #9359, .F. ) ;
#6694 = ADVANCED_FACE ( 'NONE', ( #5853 ), #12722, .F. ) ;
#6695 = CARTESIAN_POINT ( 'NONE',  ( 0.000000000000000000, 0.000000000000000000, -0.3080913168122742518 ) ) ;
#6696 = LINE ( 'NONE', #11190, #6169 ) ;
#6697 = ORIENTED_EDGE ( 'NONE', *, *, #7563, .T. ) ;
#6698 = DIRECTION ( 'NONE',  ( -0.000000000000000000, -0.000000000000000000, -1.000000000000000000 ) ) ;
#6699 = FACE_BOUND ( 'NONE', #12909, .T. ) ;
#6700 = DIRECTION ( 'NONE',  ( -0.9578262852211507639, 0.2873478855663477716, -0.000000000000000000 ) ) ;
#6701 = CARTESIAN_POINT ( 'NONE',  ( 4.000000000000000000, 2.309401076758497151, -5.000000000000000000 ) ) ;
#6702 = ORIENTED_EDGE ( 'NONE', *, *, #8817, .T. ) ;
#6703 = ADVANCED_FACE ( 'NONE', ( #11460 ), #13764, .T. ) ;
#6704 = ORIENTED_EDGE ( 'NONE', *, *, #6506, .T. ) ;
#6705 = VERTEX_POINT ( 'NONE', #2619 ) ;
#6706 = CARTESIAN_POINT ( 'NONE',  ( 1.600000000000000089, 0.000000000000000000, 7.000000000000000000 ) ) ;
#6707 = DIRECTION ( 'NONE',  ( -0.2873478855663454401, -0.9578262852211514300, 0.000000000000000000 ) ) ;
#6708 = CARTESIAN_POINT ( 'NONE',  ( 3.999999999999999112, -0.7890432684750902093, -0.04868663549882291247 ) ) ;
#6709 = DIRECTION ( 'NONE',  ( -0.2873478855663502141, -0.9578262852211498757, -4.782469237902382669E-30 ) ) ;
#6710 = CARTESIAN_POINT ( 'NONE',  ( 5.619193549421086509, 4.261310591078260046, -5.875704392893767114 ) ) ;
#6711 = CARTESIAN_POINT ( 'NONE',  ( 21.00000000000000355, 0.000000000000000000, 2.055000000000000160 ) ) ;
#6712 = DIRECTION ( 'NONE',  ( 0.2873478855663468279, 0.9578262852211509859, 0.000000000000000000 ) ) ;
#6713 = ADVANCED_FACE ( 'NONE', ( #3940 ), #4909, .F. ) ;
#6714 = ORIENTED_EDGE ( 'NONE', *, *, #6735, .F. ) ;
#6715 = CARTESIAN_POINT ( 'NONE',  ( 705.2654023280962292, 165.6605111121449738, -149.9999999999986642 ) ) ;
#6716 = PLANE ( 'NONE',  #12946 ) ;
#6717 = PRODUCT_CONTEXT ( 'NONE', #2533, 'mechanical' ) ;
#6718 = CYLINDRICAL_SURFACE ( 'NONE', #13445, 20.00000000000001776 ) ;
#6719 = ORIENTED_EDGE ( 'NONE', *, *, #1906, .T. ) ;
#6720 = ORIENTED_EDGE ( 'NONE', *, *, #11684, .F. ) ;
#6721 = FACE_OUTER_BOUND ( 'NONE', #7968, .T. ) ;
#6722 = DIRECTION ( 'NONE',  ( -1.000000000000000000, -0.000000000000000000, -0.000000000000000000 ) ) ;
#6723 = DIRECTION ( 'NONE',  ( 0.9578262852211513190, -0.2873478855663453846, -0.000000000000000000 ) ) ;
#6724 = ORIENTED_EDGE ( 'NONE', *, *, #9785, .F. ) ;
#6725 = CARTESIAN_POINT ( 'NONE',  ( 6.204460410672267834, -4.828986228461507046, -1.635950503254239408 ) ) ;
#6726 = EDGE_CURVE ( 'NONE', #13901, #2635, #9403, .T. ) ;
#6727 = VERTEX_POINT ( 'NONE', #12643 ) ;
#6728 = DIRECTION ( 'NONE',  ( 0.000000000000000000, 0.000000000000000000, 1.000000000000000000 ) ) ;
#6729 = CARTESIAN_POINT ( 'NONE',  ( 2.500000000000000000, 2.357898499370431722, -2.818925648462311528E-15 ) ) ;
#6730 = VECTOR ( 'NONE', #12697, 1000.000000000000000 ) ;
#6731 = EDGE_CURVE ( 'NONE', #11133, #8797, #1649, .T. ) ;
#6732 = LINE ( 'NONE', #4606, #8780 ) ;
#6733 = ORIENTED_EDGE ( 'NONE', *, *, #9883, .T. ) ;
#6734 = ORIENTED_EDGE ( 'NONE', *, *, #9595, .F. ) ;
#6735 = EDGE_CURVE ( 'NONE', #6439, #6968, #11677, .T. ) ;
#6736 = CARTESIAN_POINT ( 'NONE',  ( 139.8040310085880833, 355.9707293956415697, 187.0000000000000000 ) ) ;
#6737 = EDGE_CURVE ( 'NONE', #1078, #13362, #12672, .T. ) ;
#6738 = CARTESIAN_POINT ( 'NONE',  ( -1.500000000000000888, 0.000000000000000000, -5.100000000000000533 ) ) ;
#6739 = EDGE_CURVE ( 'NONE', #6877, #7500, #12869, .T. ) ;
#6740 = ORIENTED_EDGE ( 'NONE', *, *, #2127, .T. ) ;
#6741 = ORIENTED_EDGE ( 'NONE', *, *, #5278, .T. ) ;
#6742 = FACE_OUTER_BOUND ( 'NONE', #2022, .T. ) ;
#6743 = CARTESIAN_POINT ( 'NONE',  ( 642.5000000000001137, 160.0000000000000284, 210.0000059999999849 ) ) ;
#6744 = CARTESIAN_POINT ( 'NONE',  ( -9.137956343300945861, 374.5525593289318635, -184.8000000000000114 ) ) ;
#6745 = DIRECTION ( 'NONE',  ( 1.000000000000000000, 0.000000000000000000, 0.000000000000000000 ) ) ;
#6746 = ORIENTED_EDGE ( 'NONE', *, *, #7330, .F. ) ;
#6747 = CARTESIAN_POINT ( 'NONE',  ( 0.000000000000000000, 0.000000000000000000, -6.800000000000000711 ) ) ;
#6748 = ORIENTED_EDGE ( 'NONE', *, *, #14098, .F. ) ;
#6749 = ORIENTED_EDGE ( 'NONE', *, *, #6974, .T. ) ;
#6750 = CARTESIAN_POINT ( 'NONE',  ( 6.207660606242546564, -2.016205878029795784, -5.000000000000000000 ) ) ;
#6751 = ADVANCED_FACE ( 'NONE', ( #6078 ), #13994, .T. ) ;
#6752 = EDGE_CURVE ( 'NONE', #10194, #8820, #7256, .T. ) ;
#6753 = ORIENTED_EDGE ( 'NONE', *, *, #10068, .T. ) ;
#6754 = CARTESIAN_POINT ( 'NONE',  ( 641.0000000000000000, 166.0000000000000284, 187.5000000000000000 ) ) ;
#6755 = LINE ( 'NONE', #8897, #9938 ) ;
#6756 = ORIENTED_EDGE ( 'NONE', *, *, #6579, .T. ) ;
#6757 = CYLINDRICAL_SURFACE ( 'NONE', #13962, 2.649999999999985700 ) ;
#6758 = DIRECTION ( 'NONE',  ( 1.000000000000000000, 0.000000000000000000, 0.000000000000000000 ) ) ;
#6759 = EDGE_CURVE ( 'NONE', #2500, #7939, #6160, .T. ) ;
#6760 = CARTESIAN_POINT ( 'NONE',  ( 229.2257385731837473, 308.4724102386206255, 177.5999999999999091 ) ) ;
#6761 = FILL_AREA_STYLE_COLOUR ( '', #11606 ) ;
#6762 = EDGE_LOOP ( 'NONE', ( #12936, #6595, #2894, #4024 ) ) ;
#6763 = DIRECTION ( 'NONE',  ( -0.000000000000000000, -0.000000000000000000, 1.000000000000000000 ) ) ;
#6764 = AXIS2_PLACEMENT_3D ( 'NONE', #10493, #12709, #11600 ) ;
#6765 = ORIENTED_EDGE ( 'NONE', *, *, #8744, .F. ) ;
#6766 = ORIENTED_EDGE ( 'NONE', *, *, #11574, .F. ) ;
#6767 = CARTESIAN_POINT ( 'NONE',  ( 5.619193549421182432, -4.261310591078213861, -5.875704392892080463 ) ) ;
#6768 = CARTESIAN_POINT ( 'NONE',  ( 103.1953938656736227, 343.9846462189121326, -1.410137047767614819E-12 ) ) ;
#6769 = CARTESIAN_POINT ( 'NONE',  ( -20.63749999999999929, 0.000000000000000000, 0.000000000000000000 ) ) ;
#6770 = VECTOR ( 'NONE', #6015, 999.9999999999998863 ) ;
#6771 = VECTOR ( 'NONE', #12941, 1000.000000000000000 ) ;
#6772 = CARTESIAN_POINT ( 'NONE',  ( 1.600000000000000089, 0.000000000000000000, 0.000000000000000000 ) ) ;
#6773 = VECTOR ( 'NONE', #7307, 1000.000000000000114 ) ;
#6774 = DIRECTION ( 'NONE',  ( -1.000000000000000000, -0.000000000000000000, -0.000000000000000000 ) ) ;
#6775 = DIRECTION ( 'NONE',  ( -0.9578262852211517631, 0.2873478855663438858, 0.000000000000000000 ) ) ;
#6776 = DIRECTION ( 'NONE',  ( -1.000000000000000000, -0.000000000000000000, -0.000000000000000000 ) ) ;
#6777 = APPLICATION_CONTEXT ( 'automotive_design' ) ;
#6778 = ORIENTED_EDGE ( 'NONE', *, *, #4148, .T. ) ;
#6779 = SHAPE_REPRESENTATION ( 'hex flange nut gradea_iso_ISO - 4161 - M5 - N', ( #9440 ), #2159 ) ;
#6780 = CARTESIAN_POINT ( 'NONE',  ( -0.9108756637647318355, -6.979659189790606177, -6.219623095965800097 ) ) ;
#6781 = CARTESIAN_POINT ( 'NONE',  ( 636.7009106935324780, 155.5114698605638637, 211.0000000000000000 ) ) ;
#6782 = APPLICATION_PROTOCOL_DEFINITION ( 'draft international standard', 'automotive_design', 1998, #4066 ) ;
#6783 = EDGE_LOOP ( 'NONE', ( #4136, #13928, #3613, #11835 ) ) ;
#6784 =( GEOMETRIC_REPRESENTATION_CONTEXT ( 3 ) GLOBAL_UNCERTAINTY_ASSIGNED_CONTEXT ( ( #5767 ) ) GLOBAL_UNIT_ASSIGNED_CONTEXT ( ( #8862, #5905, #345 ) ) REPRESENTATION_CONTEXT ( 'NONE', 'WORKASPACE' ) );
#6785 = CARTESIAN_POINT ( 'NONE',  ( 6.746887896521065464, 3.895317543251747061, -6.526184258131188187 ) ) ;
#6786 = VECTOR ( 'NONE', #6077, 1000.000000000000000 ) ;
#6787 = ORIENTED_EDGE ( 'NONE', *, *, #14177, .T. ) ;
#6788 = ORIENTED_EDGE ( 'NONE', *, *, #12216, .F. ) ;
#6789 = CARTESIAN_POINT ( 'NONE',  ( -1.500000000000001332, 0.000000000000000000, 0.000000000000000000 ) ) ;
#6790 = CARTESIAN_POINT ( 'NONE',  ( 164.3243839102495656, 402.9042173714779551, 210.0000000000000000 ) ) ;
#6791 = DIRECTION ( 'NONE',  ( 0.2873478855663454401, 0.9578262852211514300, -3.831370512995697396E-15 ) ) ;
#6792 = EDGE_CURVE ( 'NONE', #10044, #902, #4838, .T. ) ;
#6793 = DIRECTION ( 'NONE',  ( 0.000000000000000000, 0.4999999999999990008, -0.8660254037844391517 ) ) ;
#6794 = VECTOR ( 'NONE', #9081, 1000.000000000000000 ) ;
#6795 = VECTOR ( 'NONE', #13814, 1000.000000000000000 ) ;
#6796 = CONICAL_SURFACE ( 'NONE', #4697, 5.000000000000000888, 1.047197551196600296 ) ;
#6797 = DIRECTION ( 'NONE',  ( 0.000000000000000000, 0.000000000000000000, -1.000000000000000000 ) ) ;
#6798 = VERTEX_POINT ( 'NONE', #9556 ) ;
#6799 = CARTESIAN_POINT ( 'NONE',  ( -4.000000000000000000, 2.309401076758498483, -3.433295621305379353 ) ) ;
#6800 = DIRECTION ( 'NONE',  ( 1.000000000000000000, 0.000000000000000000, 0.000000000000000000 ) ) ;
#6801 = DIRECTION ( 'NONE',  ( 1.000000000000000000, 0.000000000000000000, -0.000000000000000000 ) ) ;
#6802 = ORIENTED_EDGE ( 'NONE', *, *, #8209, .T. ) ;
#6803 = VERTEX_POINT ( 'NONE', #14056 ) ;
#6804 = CARTESIAN_POINT ( 'NONE',  ( 4.198928548860774157, -0.8158838809860124996, -3.526471437616918170 ) ) ;
#6805 = CONICAL_SURFACE ( 'NONE', #11525, 4.000000000000000000, 1.047197551196600296 ) ;
#6806 = DIRECTION ( 'NONE',  ( -0.000000000000000000, -0.000000000000000000, -1.000000000000000000 ) ) ;
#6807 = ADVANCED_FACE ( 'NONE', ( #6966 ), #1353, .T. ) ;
#6808 = LINE ( 'NONE', #6131, #5224 ) ;
#6809 = EDGE_CURVE ( 'NONE', #10412, #3419, #3526, .T. ) ;
#6810 = VERTEX_POINT ( 'NONE', #4019 ) ;
#6811 = EDGE_LOOP ( 'NONE', ( #5273, #1956, #12170, #13731 ) ) ;
#6812 = CARTESIAN_POINT ( 'NONE',  ( 609.6767525226840689, 186.8636552924789669, -187.9956429438695977 ) ) ;
#6813 = DIRECTION ( 'NONE',  ( 0.000000000000000000, 1.000000000000000000, -1.224646799147353207E-16 ) ) ;
#6814 = AXIS2_PLACEMENT_3D ( 'NONE', #5251, #11719, #5035 ) ;
#6815 = EDGE_CURVE ( 'NONE', #7275, #13362, #14272, .T. ) ;
#6816 = EDGE_CURVE ( 'NONE', #8268, #5414, #12704, .T. ) ;
#6817 = VECTOR ( 'NONE', #3382, 1000.000000000000000 ) ;
#6818 = CARTESIAN_POINT ( 'NONE',  ( 6.452281807715712247, 5.797857616946122228, 9.234669952027924180E-16 ) ) ;
#6819 = CARTESIAN_POINT ( 'NONE',  ( 1.999999999999998224, -3.464101615137772594, -3.142992957459239012 ) ) ;
#6820 = LINE ( 'NONE', #80, #285 ) ;
#6821 = ORIENTED_EDGE ( 'NONE', *, *, #1404, .T. ) ;
#6822 = ADVANCED_FACE ( 'NONE', ( #12045 ), #2914, .F. ) ;
#6823 = DIRECTION ( 'NONE',  ( -0.000000000000000000, -0.000000000000000000, 1.000000000000000000 ) ) ;
#6824 = EDGE_LOOP ( 'NONE', ( #11909, #3466, #5608, #5899 ) ) ;
#6825 = ORIENTED_EDGE ( 'NONE', *, *, #7196, .T. ) ;
#6826 = CARTESIAN_POINT ( 'NONE',  ( 610.8620436566991430, 188.5525593289318351, 169.9999999999999716 ) ) ;
#6827 = VECTOR ( 'NONE', #8383, 1000.000000000000000 ) ;
#6828 = ORIENTED_EDGE ( 'NONE', *, *, #1270, .T. ) ;
#6829 = AXIS2_PLACEMENT_3D ( 'NONE', #2710, #11777, #5019 ) ;
#6830 = DIRECTION ( 'NONE',  ( 0.000000000000000000, -1.000000000000000000, 0.000000000000000000 ) ) ;
#6831 = CARTESIAN_POINT ( 'NONE',  ( 590.0000000000000000, -9.999999999999941380, -210.0020000000000095 ) ) ;
#6832 = AXIS2_PLACEMENT_3D ( 'NONE', #14405, #6578, #13295 ) ;
#6833 = EDGE_LOOP ( 'NONE', ( #12122, #11226, #6026, #13999 ) ) ;
#6834 = CARTESIAN_POINT ( 'NONE',  ( 0.000000000000000000, 0.5192545390863916310, -1.000000000000000000 ) ) ;
#6835 = DIRECTION ( 'NONE',  ( 1.000000000000000000, 0.000000000000000000, 0.000000000000000000 ) ) ;
#6836 = AXIS2_PLACEMENT_3D ( 'NONE', #9043, #11401, #3431 ) ;
#6837 = EDGE_CURVE ( 'NONE', #2369, #1573, #182, .T. ) ;
#6838 = CARTESIAN_POINT ( 'NONE',  ( 43.50000000000000711, 4.475777889183788807E-16, -3.309499999999999886 ) ) ;
#6839 = ORIENTED_EDGE ( 'NONE', *, *, #11394, .F. ) ;
#6840 = VECTOR ( 'NONE', #13101, 1000.000000000000000 ) ;
#6841 = ADVANCED_FACE ( 'NONE', ( #14420 ), #600, .F. ) ;
#6842 = STYLED_ITEM ( 'NONE', ( #4273 ), #3907 ) ;
#6843 = CARTESIAN_POINT ( 'NONE',  ( -9.511508594537115613, 378.5275384125997107, 187.0000000000000000 ) ) ;
#6844 = PRODUCT_DEFINITION ( 'UNKNOWN', '', #13028, #14471 ) ;
#6845 = ORIENTED_EDGE ( 'NONE', *, *, #1000, .F. ) ;
#6846 = ORIENTED_EDGE ( 'NONE', *, *, #2595, .F. ) ;
#6848 = DIRECTION ( 'NONE',  ( 0.9578262852211498757, -0.2873478855663502141, 1.489419751501263930E-15 ) ) ;
#6847 = VECTOR ( 'NONE', #6280, 1000.000000000000000 ) ;
#6849 = CIRCLE ( 'NONE', #5911, 20.00000000000001776 ) ;
#6850 = DIRECTION ( 'NONE',  ( 1.000000000000000000, 2.312964634635740689E-15, 0.000000000000000000 ) ) ;
#6852 = CIRCLE ( 'NONE', #4755, 4.000000000000000000 ) ;
#6851 = CARTESIAN_POINT ( 'NONE',  ( 634.0059381729986399, 167.5000994061732911, -210.0000000000000000 ) ) ;
#6853 =( GEOMETRIC_REPRESENTATION_CONTEXT ( 3 ) GLOBAL_UNCERTAINTY_ASSIGNED_CONTEXT ( ( #10337 ) ) GLOBAL_UNIT_ASSIGNED_CONTEXT ( ( #8018, #12963, #7206 ) ) REPRESENTATION_CONTEXT ( 'NONE', 'WORKASPACE' ) );
#6854 = CARTESIAN_POINT ( 'NONE',  ( 144.7991633467111683, 386.6211705227183870, 187.0000000000000568 ) ) ;
#6855 = CARTESIAN_POINT ( 'NONE',  ( 4.000000000000000000, 2.309401076758497151, -5.000000000000000000 ) ) ;
#6856 = LINE ( 'NONE', #1317, #10138 ) ;
#6857 = DIRECTION ( 'NONE',  ( -0.000000000000000000, -0.000000000000000000, 1.000000000000000000 ) ) ;
#6858 = VERTEX_POINT ( 'NONE', #8655 ) ;
#6859 = DIRECTION ( 'NONE',  ( -0.2873478855663477716, -0.9578262852211506528, 0.000000000000000000 ) ) ;
#6860 = CARTESIAN_POINT ( 'NONE',  ( -6.781345014477444977, -3.590342129888860256, -6.122077150241852728 ) ) ;
#6861 = FACE_OUTER_BOUND ( 'NONE', #6083, .T. ) ;
#6862 = APPLICATION_PROTOCOL_DEFINITION ( 'draft international standard', 'automotive_design', 1998, #14615 ) ;
#6863 = VERTEX_POINT ( 'NONE', #1943 ) ;
#6864 = VECTOR ( 'NONE', #7938, 1000.000000000000000 ) ;
#6865 = DIRECTION ( 'NONE',  ( 1.000000000000000000, 0.000000000000000000, -0.000000000000000000 ) ) ;
#6866 = ORIENTED_EDGE ( 'NONE', *, *, #397, .T. ) ;
#6867 = ORIENTED_EDGE ( 'NONE', *, *, #10251, .F. ) ;
#6868 = DIRECTION ( 'NONE',  ( 0.000000000000000000, 0.000000000000000000, -1.000000000000000000 ) ) ;
#6869 = CARTESIAN_POINT ( 'NONE',  ( 6.196878017913830305, 3.367876570272813730, -4.166666666666666963 ) ) ;
#6870 = CARTESIAN_POINT ( 'NONE',  ( 6.533910050139692949, -2.950514251728062476, 5.110440592449057462 ) ) ;
#6871 = CIRCLE ( 'NONE', #1447, 5.249999999999976907 ) ;
#6872 = CIRCLE ( 'NONE', #9477, 6.080745460913608902 ) ;
#6873 = EDGE_CURVE ( 'NONE', #9344, #10137, #7555, .T. ) ;
#6874 = DIRECTION ( 'NONE',  ( -1.000000000000000000, 0.000000000000000000, 0.000000000000000000 ) ) ;
#6875 = STYLED_ITEM ( 'NONE', ( #460 ), #10030 ) ;
#6876 = CARTESIAN_POINT ( 'NONE',  ( 6.207530437345013752, -3.810448612250150635, -3.400109403952463971 ) ) ;
#6877 = VERTEX_POINT ( 'NONE', #5122 ) ;
#6878 = CARTESIAN_POINT ( 'NONE',  ( 448.9584422793565750, 264.0194060144110608, -210.0000000000000000 ) ) ;
#6879 = CARTESIAN_POINT ( 'NONE',  ( 610.0000000000000000, 227.4403065089105951, 187.0000000000000000 ) ) ;
#6880 = AXIS2_PLACEMENT_3D ( 'NONE', #3069, #7572, #5351 ) ;
#6881 = CARTESIAN_POINT ( 'NONE',  ( 610.8620436566991430, 230.3137853645740449, 190.0000000000000000 ) ) ;
#6882 = ADVANCED_FACE ( 'NONE', ( #11897 ), #11830, .F. ) ;
#6883 = VERTEX_POINT ( 'NONE', #9705 ) ;
#6884 = ORIENTED_EDGE ( 'NONE', *, *, #12555, .F. ) ;
#6885 = CARTESIAN_POINT ( 'NONE',  ( 627.6952049249875927, 158.0368908673054591, 210.0000120000000265 ) ) ;
#6886 = CARTESIAN_POINT ( 'NONE',  ( -0.3461262719736137305, 4.658553426539289610, -3.671615880910373608 ) ) ;
#6887 = PRODUCT_DEFINITION_FORMATION_WITH_SPECIFIED_SOURCE ( 'ANY', '', #5567, .NOT_KNOWN. ) ;
#6888 = CARTESIAN_POINT ( 'NONE',  ( 0.000000000000000000, 0.000000000000000000, 0.000000000000000000 ) ) ;
#6889 = CARTESIAN_POINT ( 'NONE',  ( 4.203935335434060505, 1.640780671294165272, -3.598452447879202598 ) ) ;
#6890 = CIRCLE ( 'NONE', #521, 3.309499999999999886 ) ;
#6891 = VERTEX_POINT ( 'NONE', #1790 ) ;
#6892 = ORIENTED_EDGE ( 'NONE', *, *, #1000, .T. ) ;
#6893 = CARTESIAN_POINT ( 'NONE',  ( 610.4437618601435815, 188.9679398019578116, -185.9079617568160074 ) ) ;
#6894 = DIRECTION ( 'NONE',  ( 1.000000000000000000, 0.000000000000000000, 0.000000000000000000 ) ) ;
#6895 = CARTESIAN_POINT ( 'NONE',  ( -4.799999999999999822, 5.878304635907294211E-16, -1.000000000000000000 ) ) ;
#6896 = DIRECTION ( 'NONE',  ( -0.000000000000000000, 1.000000000000000000, 0.000000000000000000 ) ) ;
#6897 = DIRECTION ( 'NONE',  ( 1.000000000000000000, 0.000000000000000000, 0.000000000000000000 ) ) ;
#6898 =( NAMED_UNIT ( * ) SI_UNIT ( $, .STERADIAN. ) SOLID_ANGLE_UNIT ( ) );
#6899 = EDGE_CURVE ( 'NONE', #6919, #14203, #3449, .T. ) ;
#6900 = ORIENTED_EDGE ( 'NONE', *, *, #3679, .F. ) ;
#6901 = CARTESIAN_POINT ( 'NONE',  ( -20.63749999999999929, 0.000000000000000000, 0.000000000000000000 ) ) ;
#6902 = ORIENTED_EDGE ( 'NONE', *, *, #10325, .T. ) ;
#6903 = ORIENTED_EDGE ( 'NONE', *, *, #407, .F. ) ;
#6904 = CIRCLE ( 'NONE', #1245, 2.396904916527700102 ) ;
#6905 = CARTESIAN_POINT ( 'NONE',  ( 6.541171952014627422, 2.986180817377861452, -5.112746308113085725 ) ) ;
#6906 = ORIENTED_EDGE ( 'NONE', *, *, #5170, .F. ) ;
#6907 = PRODUCT_DEFINITION_SHAPE ( 'NONE', 'NONE',  #14639 ) ;
#6908 = DIRECTION ( 'NONE',  ( -1.000000000000000000, -0.000000000000000000, -0.000000000000000000 ) ) ;
#6909 = DIRECTION ( 'NONE',  ( 0.000000000000000000, -1.000000000000000000, 0.000000000000000000 ) ) ;
#6910 = ORIENTED_EDGE ( 'NONE', *, *, #13871, .F. ) ;
#6911 = DIRECTION ( 'NONE',  ( -1.000000000000000000, -0.000000000000000000, -0.000000000000000000 ) ) ;
#6912 = CARTESIAN_POINT ( 'NONE',  ( 229.2257385731834063, 308.4724102386176128, -177.6000000000002217 ) ) ;
#6913 = DIRECTION ( 'NONE',  ( 1.000000000000000000, 0.000000000000000000, -0.000000000000000000 ) ) ;
#6914 = EDGE_CURVE ( 'NONE', #11617, #2671, #5411, .T. ) ;
#6915 = CARTESIAN_POINT ( 'NONE',  ( -4.000000000000000000, 2.309401076758498483, -5.000000000000000000 ) ) ;
#6916 = EDGE_CURVE ( 'NONE', #12480, #1630, #6089, .T. ) ;
#6917 = VERTEX_POINT ( 'NONE', #11967 ) ;
#6918 = CARTESIAN_POINT ( 'NONE',  ( 630.0000000000000000, 160.0000000000000284, 187.5000000000000000 ) ) ;
#6919 = VERTEX_POINT ( 'NONE', #11007 ) ;
#6920 = VERTEX_POINT ( 'NONE', #1862 ) ;
#6921 = CARTESIAN_POINT ( 'NONE',  ( 1.600000000000000089, 0.000000000000000000, 0.000000000000000000 ) ) ;
#6922 = ADVANCED_FACE ( 'NONE', ( #6375 ), #8220, .T. ) ;
#6923 = EDGE_CURVE ( 'NONE', #14237, #11464, #73, .T. ) ;
#6924 = CARTESIAN_POINT ( 'NONE',  ( -1.250000000000000000, -6.429618962271402616, 0.000000000000000000 ) ) ;
#6925 = DIRECTION ( 'NONE',  ( -0.000000000000000000, -0.000000000000000000, 1.000000000000000000 ) ) ;
#6926 = EDGE_CURVE ( 'NONE', #10699, #293, #9985, .T. ) ;
#6927 = DIRECTION ( 'NONE',  ( -0.2873478855663453846, -0.9578262852211513190, 0.000000000000000000 ) ) ;
#6928 = CARTESIAN_POINT ( 'NONE',  ( 5.200000000000002842, 3.306546357697854226E-16, 2.700000000000000622 ) ) ;
#6929 = CARTESIAN_POINT ( 'NONE',  ( -6.831985876597697072, 3.295913427296342402, -6.443925148804115821 ) ) ;
#6930 = CARTESIAN_POINT ( 'NONE',  ( 448.9584422793565750, 264.0194060144110608, 187.0000000000000000 ) ) ;
#6931 = EDGE_LOOP ( 'NONE', ( #11681, #3335, #3058, #12599 ) ) ;
#6932 = CARTESIAN_POINT ( 'NONE',  ( 145.1678582058265192, 408.6511750828049117, -210.0000000000000000 ) ) ;
#6933 = CARTESIAN_POINT ( 'NONE',  ( 228.5935732249376997, 306.3651924111334779, 177.6000000000001648 ) ) ;
#6934 = CARTESIAN_POINT ( 'NONE',  ( 610.1557962250110450, 190.0426856094898085, 186.7771368031600048 ) ) ;
#6935 = ITEM_DEFINED_TRANSFORMATION ( 'NONE', 'NONE', #13486,  #9440 ) ;
#6936 = ORIENTED_EDGE ( 'NONE', *, *, #1320, .F. ) ;
#6937 = DIRECTION ( 'NONE',  ( -1.000000000000000000, -0.000000000000000000, -0.000000000000000000 ) ) ;
#6938 = EDGE_LOOP ( 'NONE', ( #1469, #6704, #602, #10994 ) ) ;
#6939 = ORIENTED_EDGE ( 'NONE', *, *, #3409, .T. ) ;
#6940 = CARTESIAN_POINT ( 'NONE',  ( 1.500000000000001332, 0.000000000000000000, 0.000000000000000000 ) ) ;
#6941 = DIRECTION ( 'NONE',  ( -1.000000000000000000, 0.000000000000000000, 0.000000000000000000 ) ) ;
#6942 = ADVANCED_FACE ( 'NONE', ( #5895 ), #4876, .F. ) ;
#6943 = CARTESIAN_POINT ( 'NONE',  ( 629.0000000000000000, 166.0000000000000284, 187.5000000000000000 ) ) ;
#6944 = CARTESIAN_POINT ( 'NONE',  ( 33.50000000000000000, 0.000000000000000000, 0.000000000000000000 ) ) ;
#6945 = CARTESIAN_POINT ( 'NONE',  ( 0.000000000000000000, 0.000000000000000000, 0.000000000000000000 ) ) ;
#6946 = VERTEX_POINT ( 'NONE', #1390 ) ;
#6947 = ADVANCED_FACE ( 'NONE', ( #338 ), #13303, .F. ) ;
#6948 = FACE_OUTER_BOUND ( 'NONE', #777, .T. ) ;
#6949 = CARTESIAN_POINT ( 'NONE',  ( -0.3198814748697807464, -4.434118497892185040, -0.3507732604232532969 ) ) ;
#6950 = DIRECTION ( 'NONE',  ( -0.9237280213470682178, -0.3830490080632377725, 0.000000000000000000 ) ) ;
#6951 = ADVANCED_FACE ( 'NONE', ( #4734 ), #6589, .F. ) ;
#6952 = LINE ( 'NONE', #13372, #3785 ) ;
#6953 = ORIENTED_EDGE ( 'NONE', *, *, #12311, .T. ) ;
#6954 = ORIENTED_EDGE ( 'NONE', *, *, #9691, .T. ) ;
#6955 = FACE_OUTER_BOUND ( 'NONE', #9940, .T. ) ;
#6956 = LINE ( 'NONE', #11451, #13205 ) ;
#6957 = CARTESIAN_POINT ( 'NONE',  ( -6.500000000000000000, 3.752776749732564809, -0.7999999999999969358 ) ) ;
#6958 = CARTESIAN_POINT ( 'NONE',  ( -4.207491450040567571, 2.029819825146470524, -3.671670828759566074 ) ) ;
#6959 = SHAPE_REPRESENTATION ( 'roller', ( #9440 ), #6853 ) ;
#6960 = B_SPLINE_CURVE_WITH_KNOTS ( 'NONE', 3,
 ( #5467, #14468, #11963, #2826, #11208, #1856, #6646, #11139 ),
 .UNSPECIFIED., .F., .F.,
 ( 4, 2, 2, 4 ),
 ( 0.005725059856848645212, 0.006314084072593634418, 0.006903108288338624492, 0.008081156719828603771 ),
 .UNSPECIFIED. ) ;
#6961 = ORIENTED_EDGE ( 'NONE', *, *, #3278, .T. ) ;
#6962 = EDGE_LOOP ( 'NONE', ( #3595, #13163, #10639, #4945 ) ) ;
#6963 = DIRECTION ( 'NONE',  ( 0.000000000000000000, 0.000000000000000000, 1.000000000000000000 ) ) ;
#6964 = FACE_OUTER_BOUND ( 'NONE', #891, .T. ) ;
#6965 = CARTESIAN_POINT ( 'NONE',  ( 639.4338945024659324, 161.8386352387035743, -210.0000000000000000 ) ) ;
#6966 = FACE_OUTER_BOUND ( 'NONE', #531, .T. ) ;
#6967 = DIRECTION ( 'NONE',  ( -0.000000000000000000, -0.000000000000000000, 1.000000000000000000 ) ) ;
#6968 = VERTEX_POINT ( 'NONE', #1321 ) ;
#6969 = FACE_OUTER_BOUND ( 'NONE', #3059, .T. ) ;
#6970 = ORIENTED_EDGE ( 'NONE', *, *, #7165, .T. ) ;
#6971 = ORIENTED_EDGE ( 'NONE', *, *, #6645, .T. ) ;
#6972 = CARTESIAN_POINT ( 'NONE',  ( 6.390821132688881967, 3.013780087859768919, -5.000000000000000000 ) ) ;
#6973 = CARTESIAN_POINT ( 'NONE',  ( 112.9652219749295341, 376.5507399164317803, -210.0000000000000000 ) ) ;
#6974 = EDGE_CURVE ( 'NONE', #12815, #11448, #13891, .T. ) ;
#6975 = DIRECTION ( 'NONE',  ( -0.9237280213470676626, -0.3830490080632388272, 0.000000000000000000 ) ) ;
#6976 = ORIENTED_EDGE ( 'NONE', *, *, #11248, .T. ) ;
#6977 = DIRECTION ( 'NONE',  ( -0.9578262852211507639, 0.2873478855663477716, 0.000000000000000000 ) ) ;
#6978 = PLANE ( 'NONE',  #8009 ) ;
#6979 = FACE_BOUND ( 'NONE', #6576, .T. ) ;
#6980 = ORIENTED_EDGE ( 'NONE', *, *, #1273, .T. ) ;
#6981 = DIRECTION ( 'NONE',  ( -0.000000000000000000, 0.000000000000000000, -1.000000000000000000 ) ) ;
#6982 = ORIENTED_EDGE ( 'NONE', *, *, #12467, .F. ) ;
#6983 = ORIENTED_EDGE ( 'NONE', *, *, #1765, .T. ) ;
#6984 = DIRECTION ( 'NONE',  ( 3.340694023494469140E-16, -4.069768234201303760E-15, -1.000000000000000000 ) ) ;
#6985 = LINE ( 'NONE', #2337, #1414 ) ;
#6986 = ADVANCED_FACE ( 'NONE', ( #3691 ), #12181, .F. ) ;
#6987 = CARTESIAN_POINT ( 'NONE',  ( -8.074769166705394241, 378.0965165842501392, 190.0000000000000000 ) ) ;
#6988 = ORIENTED_EDGE ( 'NONE', *, *, #704, .T. ) ;
#6989 = FACE_BOUND ( 'NONE', #2231, .T. ) ;
#6990 = EDGE_CURVE ( 'NONE', #7989, #3531, #3462, .T. ) ;
#6991 = CARTESIAN_POINT ( 'NONE',  ( -6.500000000000000000, -3.155218591052673549, -0.5622968210053901350 ) ) ;
#6992 = FACE_OUTER_BOUND ( 'NONE', #6994, .T. ) ;
#6993 = CARTESIAN_POINT ( 'NONE',  ( 2.742827927723449299, 3.035229711104609596, -3.433252694550591233 ) ) ;
#6994 = EDGE_LOOP ( 'NONE', ( #5589, #396, #6866, #2359 ) ) ;
#6995 = EDGE_CURVE ( 'NONE', #12155, #2217, #13639, .T. ) ;
#6996 = CARTESIAN_POINT ( 'NONE',  ( 10.00000000000000000, -10.00000000000000000, -210.0020000000000095 ) ) ;
#6997 = CARTESIAN_POINT ( 'NONE',  ( -4.424031367838992423, -4.951337798339370266, -6.056431503346042078 ) ) ;
#6998 = CARTESIAN_POINT ( 'NONE',  ( 6.534838248920896930, 2.951765777552409986, -5.112608298763837489 ) ) ;
#6999 = CONTEXT_DEPENDENT_SHAPE_REPRESENTATION ( #11871, #4073 ) ;
#7000 = VERTEX_POINT ( 'NONE', #973 ) ;
#7002 = EDGE_CURVE ( 'NONE', #4863, #13301, #2070, .T. ) ;
#7001 = CARTESIAN_POINT ( 'NONE',  ( 6.541334450618641938, 2.987059910623325987, 5.112749838330405083 ) ) ;
#7003 = ORIENTED_EDGE ( 'NONE', *, *, #4054, .F. ) ;
#7004 = ORIENTED_EDGE ( 'NONE', *, *, #11417, .F. ) ;
#7005 = DIRECTION ( 'NONE',  ( 0.2873478855663503251, 0.9578262852211498757, 0.000000000000000000 ) ) ;
#7006 = PRESENTATION_LAYER_ASSIGNMENT (  '', '', ( #1105 ) ) ;
#7008 = DIRECTION ( 'NONE',  ( 0.000000000000000000, 0.000000000000000000, -1.000000000000000000 ) ) ;
#7007 = VECTOR ( 'NONE', #2413, 1000.000000000000000 ) ;
#7009 = LINE ( 'NONE', #4666, #8978 ) ;
#7010 = LINE ( 'NONE', #10267, #11137 ) ;
#7011 = ORIENTED_EDGE ( 'NONE', *, *, #6012, .T. ) ;
#7012 = EDGE_CURVE ( 'NONE', #681, #8674, #11088, .T. ) ;
#7013 = CIRCLE ( 'NONE', #6086, 0.1000000000000002554 ) ;
#7014 = ADVANCED_FACE ( 'NONE', ( #11495 ), #5753, .F. ) ;
#7015 = CARTESIAN_POINT ( 'NONE',  ( 708.1388811837593948, 164.7984674554466835, -177.6000000000002217 ) ) ;
#7016 = DIRECTION ( 'NONE',  ( -1.000000000000000000, 0.000000000000000000, 0.000000000000000000 ) ) ;
#7017 = DIRECTION ( 'NONE',  ( 0.000000000000000000, 0.000000000000000000, -1.000000000000000000 ) ) ;
#7019 = ADVANCED_FACE ( 'NONE', ( #8171 ), #11742, .T. ) ;
#7018 = CARTESIAN_POINT ( 'NONE',  ( 0.000000000000000000, 4.898587196589412829E-16, -4.000000000000000000 ) ) ;
#7020 = EDGE_LOOP ( 'NONE', ( #13518, #10734, #802, #11658 ) ) ;
#7021 = ORIENTED_EDGE ( 'NONE', *, *, #4794, .F. ) ;
#7022 = CARTESIAN_POINT ( 'NONE',  ( 636.7717819724297215, 155.3244477714206653, -222.5000000000000000 ) ) ;
#7023 = DIRECTION ( 'NONE',  ( 0.000000000000000000, -0.5000000000000013323, -0.8660254037844380415 ) ) ;
#7024 = ADVANCED_BREP_SHAPE_REPRESENTATION ( '', ( #12291, #9440 ), #2159 ) ;
#7025 = CARTESIAN_POINT ( 'NONE',  ( -10.00000000000000000, 0.000000000000000000, 210.0000000000000000 ) ) ;
#7026 = AXIS2_PLACEMENT_3D ( 'NONE', #1083, #10022, #5459 ) ;
#7027 = VECTOR ( 'NONE', #7915, 1000.000000000000000 ) ;
#7028 = AXIS2_PLACEMENT_3D ( 'NONE', #2830, #12940, #1727 ) ;
#7029 = ORIENTED_EDGE ( 'NONE', *, *, #11207, .T. ) ;
#7030 = ORIENTED_EDGE ( 'NONE', *, *, #10167, .T. ) ;
#7031 = CARTESIAN_POINT ( 'NONE',  ( 610.1840840298345938, 189.9120001624725376, -186.6958543268122526 ) ) ;
#7032 = CARTESIAN_POINT ( 'NONE',  ( 4.000000000000000000, -2.309401076758514915, -5.000000000000000000 ) ) ;
#7033 = CARTESIAN_POINT ( 'NONE',  ( 6.534533895392296010, 5.902695350657467088, 8.411391101939246700E-15 ) ) ;
#7034 = DIRECTION ( 'NONE',  ( 0.000000000000000000, 0.000000000000000000, 1.000000000000000000 ) ) ;
#7035 = CARTESIAN_POINT ( 'NONE',  ( -2.804994570502171047, -3.229033611042465335, -3.526374918436838701 ) ) ;
#7036 = ORIENTED_EDGE ( 'NONE', *, *, #5914, .T. ) ;
#7037 = AXIS2_PLACEMENT_3D ( 'NONE', #14015, #2780, #1680 ) ;
#7038 = FACE_OUTER_BOUND ( 'NONE', #11795, .T. ) ;
#7039 = AXIS2_PLACEMENT_3D ( 'NONE', #2153, #3567, #6800 ) ;
#7040 = ORIENTED_EDGE ( 'NONE', *, *, #8420, .T. ) ;
#7041 = ORIENTED_EDGE ( 'NONE', *, *, #6173, .F. ) ;
#7042 = DIRECTION ( 'NONE',  ( 0.3543563944859323689, -0.9351104457158684324, 0.000000000000000000 ) ) ;
#7043 = AXIS2_PLACEMENT_3D ( 'NONE', #7412, #8807, #3052 ) ;
#7044 = DIRECTION ( 'NONE',  ( 0.000000000000000000, 0.000000000000000000, -1.000000000000000000 ) ) ;
#7045 = CARTESIAN_POINT ( 'NONE',  ( 33.50000000000000000, 0.000000000000000000, 0.000000000000000000 ) ) ;
#7046 = AXIS2_PLACEMENT_3D ( 'NONE', #6426, #8701, #7229 ) ;
#7047 = ORIENTED_EDGE ( 'NONE', *, *, #7972, .T. ) ;
#7048 = CARTESIAN_POINT ( 'NONE',  ( 611.4942090049449916, 232.4210031920597999, 184.7999999999999829 ) ) ;
#7049 = LINE ( 'NONE', #250, #5651 ) ;
#7050 = CARTESIAN_POINT ( 'NONE',  ( 6.244889965166093404, -4.918546365148220190, 1.691415889817839968 ) ) ;
#7051 = CARTESIAN_POINT ( 'NONE',  ( 0.1920286436967153787, 0.000000000000000000, 0.000000000000000000 ) ) ;
#7052 = VERTEX_POINT ( 'NONE', #8041 ) ;
#7053 = COLOUR_RGB ( '',0.8941176470588234615, 0.8941176470588234615, 0.8941176470588234615 ) ;
#7054 = DIRECTION ( 'NONE',  ( 0.000000000000000000, 0.8660254037844375974, -0.5000000000000019984 ) ) ;
#7055 = EDGE_LOOP ( 'NONE', ( #8356, #2793, #14278, #1756 ) ) ;
#7056 = EDGE_CURVE ( 'NONE', #3815, #4304, #5400, .T. ) ;
#7057 = AXIS2_PLACEMENT_3D ( 'NONE', #3295, #3219, #8769 ) ;
#7058 = VECTOR ( 'NONE', #12003, 1000.000000000000000 ) ;
#7059 = ADVANCED_FACE ( 'NONE', ( #190 ), #10588, .T. ) ;
#7060 = EDGE_LOOP ( 'NONE', ( #6596, #13558, #10966, #4405, #6631, #461, #1479, #11941 ) ) ;
#7061 = CYLINDRICAL_SURFACE ( 'NONE', #13883, 7.000000000000000000 ) ;
#7062 = APPLICATION_CONTEXT ( 'automotive_design' ) ;
#7063 = DIRECTION ( 'NONE',  ( -1.000000000000000000, 0.000000000000000000, 0.000000000000000000 ) ) ;
#7064 = CARTESIAN_POINT ( 'NONE',  ( 631.0000000000000000, 164.0000000000000284, -233.5000000000000000 ) ) ;
#7065 = ORIENTED_EDGE ( 'NONE', *, *, #10530, .T. ) ;
#7066 = DIRECTION ( 'NONE',  ( 0.1305261922200524616, -0.9914448613738103822, 0.000000000000000000 ) ) ;
#7067 = CONICAL_SURFACE ( 'NONE', #2361, 4.000000000000000000, 0.8911886515913786111 ) ;
#7068 = CIRCLE ( 'NONE', #4489, 4.000000000000000000 ) ;
#7069 = CARTESIAN_POINT ( 'NONE',  ( -6.500000000000000000, -3.752776749732573247, -0.8000000000000003775 ) ) ;
#7070 = CYLINDRICAL_SURFACE ( 'NONE', #5653, 2.649999999999985700 ) ;
#7071 = ORIENTED_EDGE ( 'NONE', *, *, #11623, .F. ) ;
#7072 = CARTESIAN_POINT ( 'NONE',  ( 642.0000000000000000, 235.0000000000000284, -233.5000000000000000 ) ) ;
#7073 = MANIFOLD_SOLID_BREP ( 'FlangeHexFillet', #14227 ) ;
#7074 = CARTESIAN_POINT ( 'NONE',  ( 610.0000000000000000, 145.0000000000000568, -210.0000000000000000 ) ) ;
#7075 = EDGE_LOOP ( 'NONE', ( #7518, #9493, #8924, #4111 ) ) ;
#7076 = AXIS2_PLACEMENT_3D ( 'NONE', #12033, #11951, #7624 ) ;
#7077 = EDGE_CURVE ( 'NONE', #13548, #9831, #956, .T. ) ;
#7078 = CIRCLE ( 'NONE', #1669, 5.100000000000000533 ) ;
#7079 = CARTESIAN_POINT ( 'NONE',  ( 6.207682235858348108, 2.016324304256104760, 4.999999999999999112 ) ) ;
#7080 = ORIENTED_EDGE ( 'NONE', *, *, #9309, .T. ) ;
#7081 = ORIENTED_EDGE ( 'NONE', *, *, #6511, .F. ) ;
#7082 = DIRECTION ( 'NONE',  ( 0.000000000000000000, 0.000000000000000000, 1.000000000000000000 ) ) ;
#7083 = CARTESIAN_POINT ( 'NONE',  ( -1.098735407080685844, 7.248058225761802476, -6.326622577871337860 ) ) ;
#7084 = AXIS2_PLACEMENT_3D ( 'NONE', #3515, #1446, #5952 ) ;
#7085 = AXIS2_PLACEMENT_3D ( 'NONE', #267, #4808, #14021 ) ;
#7086 = CARTESIAN_POINT ( 'NONE',  ( 142.4540310085880606, 355.9707293956415697, 187.0000000000000000 ) ) ;
#7087 = EDGE_CURVE ( 'NONE', #10436, #1995, #1608, .T. ) ;
#7088 = CIRCLE ( 'NONE', #10391, 2.649999999999985700 ) ;
#7089 = CARTESIAN_POINT ( 'NONE',  ( 443.6584422793565636, 264.0194060144110608, -187.0000000000000000 ) ) ;
#7090 = DIRECTION ( 'NONE',  ( 1.000000000000000000, 0.000000000000000000, 0.000000000000000000 ) ) ;
#7091 = ORIENTED_EDGE ( 'NONE', *, *, #14497, .F. ) ;
#7092 = AXIS2_PLACEMENT_3D ( 'NONE', #6389, #6678, #13313 ) ;
#7093 =( GEOMETRIC_REPRESENTATION_CONTEXT ( 3 ) GLOBAL_UNCERTAINTY_ASSIGNED_CONTEXT ( ( #1766 ) ) GLOBAL_UNIT_ASSIGNED_CONTEXT ( ( #1303, #13492, #28 ) ) REPRESENTATION_CONTEXT ( 'NONE', 'WORKASPACE' ) );
#7094 = DIRECTION ( 'NONE',  ( 0.9578262852211508749, -0.2873478855663470499, 0.000000000000000000 ) ) ;
#7095 = PLANE ( 'NONE',  #14575 ) ;
#7096 = DIRECTION ( 'NONE',  ( 1.000000000000000000, 0.000000000000000000, 0.000000000000000000 ) ) ;
#7097 = ADVANCED_FACE ( 'NONE', ( #6199 ), #8155, .F. ) ;
#7098 = CARTESIAN_POINT ( 'NONE',  ( 6.534838248920897819, 2.951765777552412651, 5.112608298763836601 ) ) ;
#7099 = VERTEX_POINT ( 'NONE', #12837 ) ;
#7100 = ORIENTED_EDGE ( 'NONE', *, *, #3002, .T. ) ;
#7101 = AXIS2_PLACEMENT_3D ( 'NONE', #11138, #10854, #5254 ) ;
#7102 = DIRECTION ( 'NONE',  ( -0.9237280213470676626, -0.3830490080632388272, 0.000000000000000000 ) ) ;
#7103 = LINE ( 'NONE', #9393, #5001 ) ;
#7104 = AXIS2_PLACEMENT_3D ( 'NONE', #6736, #5556, #10211 ) ;
#7105 = MANIFOLD_SOLID_BREP ( 'Body', #14463 ) ;
#7106 = DIRECTION ( 'NONE',  ( 0.000000000000000000, 0.000000000000000000, -1.000000000000000000 ) ) ;
#7107 = ADVANCED_FACE ( 'NONE', ( #3169 ), #6335, .F. ) ;
#7108 = ADVANCED_FACE ( 'NONE', ( #4350 ), #9743, .T. ) ;
#7109 =( GEOMETRIC_REPRESENTATION_CONTEXT ( 3 ) GLOBAL_UNCERTAINTY_ASSIGNED_CONTEXT ( ( #9312 ) ) GLOBAL_UNIT_ASSIGNED_CONTEXT ( ( #5222, #8604, #13180 ) ) REPRESENTATION_CONTEXT ( 'NONE', 'WORKASPACE' ) );
#7110 = ORIENTED_EDGE ( 'NONE', *, *, #4448, .T. ) ;
#7111 = EDGE_CURVE ( 'NONE', #10050, #10093, #6555, .T. ) ;
#7112 = PRODUCT_RELATED_PRODUCT_CATEGORY ( 'part', '', ( #8160 ) ) ;
#7113 = VECTOR ( 'NONE', #7709, 1000.000000000000000 ) ;
#7114 = FACE_BOUND ( 'NONE', #3875, .T. ) ;
#7115 = CARTESIAN_POINT ( 'NONE',  ( 610.3730626637085379, 189.1846890958936740, -186.1333820183295984 ) ) ;
#7116 = CARTESIAN_POINT ( 'NONE',  ( 3.983107665916332252, -5.570601890521292177, -6.171481112545254000 ) ) ;
#7117 = DIRECTION ( 'NONE',  ( 1.000000000000000000, 0.000000000000000000, 0.000000000000000000 ) ) ;
#7118 = DIRECTION ( 'NONE',  ( -1.000000000000000000, 0.000000000000000000, 0.000000000000000000 ) ) ;
#7119 =( LENGTH_UNIT ( ) NAMED_UNIT ( * ) SI_UNIT ( .MILLI., .METRE. ) );
#7120 = PRODUCT_DEFINITION_SHAPE ( 'NONE', 'NONE',  #14620 ) ;
#7121 = ORIENTED_EDGE ( 'NONE', *, *, #31, .F. ) ;
#7122 = AXIS2_PLACEMENT_3D ( 'NONE', #5838, #11661, #9388 ) ;
#7123 = LINE ( 'NONE', #9491, #5884 ) ;
#7124 = VERTEX_POINT ( 'NONE', #8622 ) ;
#7125 = ORIENTED_EDGE ( 'NONE', *, *, #9862, .F. ) ;
#7126 = DIRECTION ( 'NONE',  ( -0.000000000000000000, -0.000000000000000000, -1.000000000000000000 ) ) ;
#7127 = CIRCLE ( 'NONE', #1938, 2.499999999999946709 ) ;
#7128 = DIRECTION ( 'NONE',  ( 0.000000000000000000, 1.000000000000000000, 0.000000000000000000 ) ) ;
#7129 = CARTESIAN_POINT ( 'NONE',  ( -31.74999999999995737, 3.061616997868383634E-16, -2.500000000000000444 ) ) ;
#7130 = DIRECTION ( 'NONE',  ( 0.000000000000000000, 0.000000000000000000, -1.000000000000000000 ) ) ;
#7131 = AXIS2_PLACEMENT_3D ( 'NONE', #5990, #1492, #355 ) ;
#7132 = ORIENTED_EDGE ( 'NONE', *, *, #12602, .T. ) ;
#7133 = FACE_OUTER_BOUND ( 'NONE', #2257, .T. ) ;
#7134 = CARTESIAN_POINT ( 'NONE',  ( 6.838238910409970117, -3.993980678889271552, -6.572970348078615466 ) ) ;
#7135 = LINE ( 'NONE', #10743, #1811 ) ;
#7136 = CARTESIAN_POINT ( 'NONE',  ( 6.080745460913608902, 0.5192545390863916310, -1.000000000000000000 ) ) ;
#7137 = PRESENTATION_STYLE_ASSIGNMENT (( #10679 ) ) ;
#7138 = VERTEX_POINT ( 'NONE', #8908 ) ;
#7139 = EDGE_CURVE ( 'NONE', #9301, #4023, #854, .T. ) ;
#7140 = FACE_OUTER_BOUND ( 'NONE', #9708, .T. ) ;
#7141 = EDGE_LOOP ( 'NONE', ( #10421, #7960, #9453, #1654, #1292 ) ) ;
#7142 = EDGE_CURVE ( 'NONE', #10448, #2847, #12154, .T. ) ;
#7143 = DIRECTION ( 'NONE',  ( -0.000000000000000000, -0.000000000000000000, 1.000000000000000000 ) ) ;
#7144 = DIRECTION ( 'NONE',  ( -9.028085479645851510E-15, -3.009361826548617065E-14, -1.000000000000000000 ) ) ;
#7145 = AXIS2_PLACEMENT_3D ( 'NONE', #4549, #2304, #6686 ) ;
#7146 = CARTESIAN_POINT ( 'NONE',  ( 0.6666666666666689611, 4.233901974057261874, -3.300726591567082480 ) ) ;
#7147 = CLOSED_SHELL ( 'NONE', ( #2861, #8345, #12139, #3514, #787, #10970, #6664, #1762 ) ) ;
#7148 = VERTEX_POINT ( 'NONE', #3230 ) ;
#7149 = CARTESIAN_POINT ( 'NONE',  ( 609.6698590453944462, 186.8406770348469195, 188.0140793454688151 ) ) ;
#7150 = EDGE_CURVE ( 'NONE', #5419, #9344, #2193, .T. ) ;
#7151 = CARTESIAN_POINT ( 'NONE',  ( 0.000000000000000000, 0.000000000000000000, 0.000000000000000000 ) ) ;
#7152 = CARTESIAN_POINT ( 'NONE',  ( -5.357619327558936585E-16, 7.505553499465137612, -6.064240316920400886 ) ) ;
#7153 = ORIENTED_EDGE ( 'NONE', *, *, #561, .F. ) ;
#7154 = CARTESIAN_POINT ( 'NONE',  ( 6.445379721942640749, -2.463581311471621849, -5.110653333236677476 ) ) ;
#7155 = MANIFOLD_SOLID_BREP ( 'Cut-Extrude1', #7147 ) ;
#7156 = PLANE ( 'NONE',  #9132 ) ;
#7157 = ORIENTED_EDGE ( 'NONE', *, *, #2864, .T. ) ;
#7158 = CARTESIAN_POINT ( 'NONE',  ( 1.600000000000000089, 0.000000000000000000, 0.000000000000000000 ) ) ;
#7159 = ORIENTED_EDGE ( 'NONE', *, *, #3873, .T. ) ;
#7160 = ORIENTED_EDGE ( 'NONE', *, *, #2207, .F. ) ;
#7161 = CARTESIAN_POINT ( 'NONE',  ( 139.8040310085880833, 355.9707293956415697, -187.0000000000000000 ) ) ;
#7162 = DIRECTION ( 'NONE',  ( -0.9578262852211498757, 0.2873478855663503251, -1.198990317802636355E-15 ) ) ;
#7163 = CARTESIAN_POINT ( 'NONE',  ( 6.534838248920896930, 2.951765777552409986, -5.112608298763837489 ) ) ;
#7164 = EDGE_CURVE ( 'NONE', #2958, #8217, #7854, .T. ) ;
#7165 = EDGE_CURVE ( 'NONE', #4684, #12841, #10920, .T. ) ;
#7166 = EDGE_CURVE ( 'NONE', #4609, #1573, #8466, .T. ) ;
#7167 = CARTESIAN_POINT ( 'NONE',  ( 708.1388811837593948, 164.7984674554466835, -179.7999999999999545 ) ) ;
#7168 = DIRECTION ( 'NONE',  ( 1.000000000000000000, 0.000000000000000000, 0.000000000000000000 ) ) ;
#7169 = ORIENTED_EDGE ( 'NONE', *, *, #9164, .F. ) ;
#7170 = PLANE ( 'NONE',  #6570 ) ;
#7171 = CARTESIAN_POINT ( 'NONE',  ( 1.083333333333332593, -6.880090707843051767, -5.848636054922041083 ) ) ;
#7172 = DIRECTION ( 'NONE',  ( -1.000000000000000000, 0.000000000000000000, 0.000000000000000000 ) ) ;
#7173 = CARTESIAN_POINT ( 'NONE',  ( 0.000000000000000000, 0.000000000000000000, 0.000000000000000000 ) ) ;
#7174 = ORIENTED_EDGE ( 'NONE', *, *, #7699, .F. ) ;
#7175 = ORIENTED_EDGE ( 'NONE', *, *, #507, .F. ) ;
#7176 = CARTESIAN_POINT ( 'NONE',  ( 0.000000000000000000, 0.000000000000000000, 0.000000000000000000 ) ) ;
#7177 = LINE ( 'NONE', #5926, #3782 ) ;
#7178 = CARTESIAN_POINT ( 'NONE',  ( -10.00000000000000000, 10.00000000000000178, -190.0000000000000000 ) ) ;
#7179 = EDGE_CURVE ( 'NONE', #2008, #8976, #9873, .T. ) ;
#7180 = DIRECTION ( 'NONE',  ( -0.2873478855663437748, -0.9578262852211518741, 0.000000000000000000 ) ) ;
#7181 = VERTEX_POINT ( 'NONE', #1152 ) ;
#7182 = DIRECTION ( 'NONE',  ( -0.000000000000000000, 0.000000000000000000, -1.000000000000000000 ) ) ;
#7183 = CARTESIAN_POINT ( 'NONE',  ( 6.466260427357664931, -2.904280683598016832, -5.030361703432624232 ) ) ;
#7184 = CARTESIAN_POINT ( 'NONE',  ( -8.505790995054899994, 376.6597771564184427, 184.8000000000000398 ) ) ;
#7185 = ADVANCED_FACE ( 'NONE', ( #2554 ), #98, .F. ) ;
#7186 = DIRECTION ( 'NONE',  ( 0.000000000000000000, 0.000000000000000000, -1.000000000000000000 ) ) ;
#7187 = CARTESIAN_POINT ( 'NONE',  ( 629.0000000000000000, 154.0000000000000284, -187.5000000000000000 ) ) ;
#7188 = DIRECTION ( 'NONE',  ( 0.9578262852211485434, -0.2873478855663546550, 0.000000000000000000 ) ) ;
#7189 = FILL_AREA_STYLE ('',( #10581 ) ) ;
#7190 = EDGE_LOOP ( 'NONE', ( #4901, #97, #9526, #5358 ) ) ;
#7191 = EDGE_CURVE ( 'NONE', #4012, #4648, #4957, .T. ) ;
#7192 = CARTESIAN_POINT ( 'NONE',  ( 0.6640947660595348800, -4.471078309994175548, -3.602146406945708090 ) ) ;
#7193 = EDGE_LOOP ( 'NONE', ( #13840, #11052, #6953, #8078 ) ) ;
#7194 = EDGE_LOOP ( 'NONE', ( #616, #1743, #14282, #36 ) ) ;
#7195 = DIRECTION ( 'NONE',  ( 0.000000000000000000, 0.000000000000000000, 1.000000000000000000 ) ) ;
#7196 = EDGE_CURVE ( 'NONE', #11464, #8256, #6441, .T. ) ;
#7197 = EDGE_CURVE ( 'NONE', #7500, #8478, #13715, .T. ) ;
#7198 = DIRECTION ( 'NONE',  ( -0.2873478855663461062, -0.9578262852211510969, 6.938893903907199190E-15 ) ) ;
#7199 = DIRECTION ( 'NONE',  ( 1.000000000000000000, -3.469446951953611033E-15, 0.000000000000000000 ) ) ;
#7200 = CYLINDRICAL_SURFACE ( 'NONE', #2054, 4.799999999999968736 ) ;
#7201 = VERTEX_POINT ( 'NONE', #6918 ) ;
#7202 = DIRECTION ( 'NONE',  ( 1.000000000000000000, 0.000000000000000000, 0.000000000000000000 ) ) ;
#7203 = FACE_OUTER_BOUND ( 'NONE', #3715, .T. ) ;
#7204 = CARTESIAN_POINT ( 'NONE',  ( 6.244004651191001010, -4.178905357954648458, 2.972460101650454600 ) ) ;
#7205 =( NAMED_UNIT ( * ) PLANE_ANGLE_UNIT ( ) SI_UNIT ( $, .RADIAN. ) );
#7206 =( NAMED_UNIT ( * ) SI_UNIT ( $, .STERADIAN. ) SOLID_ANGLE_UNIT ( ) );
#7207 = ORIENTED_EDGE ( 'NONE', *, *, #2232, .T. ) ;
#7208 = ADVANCED_FACE ( 'NONE', ( #7945 ), #8989, .F. ) ;
#7209 = EDGE_CURVE ( 'NONE', #2165, #2500, #5585, .T. ) ;
#7210 = CARTESIAN_POINT ( 'NONE',  ( -20.63749999999999929, 0.000000000000000000, -5.000000000000000000 ) ) ;
#7211 = ORIENTED_EDGE ( 'NONE', *, *, #8372, .T. ) ;
#7212 = EDGE_CURVE ( 'NONE', #7913, #2553, #3446, .T. ) ;
#7213 = CARTESIAN_POINT ( 'NONE',  ( 650.0000000000000000, 175.0000000000000568, -210.0000000000000000 ) ) ;
#7214 = DIRECTION ( 'NONE',  ( -1.000000000000000000, 0.000000000000000000, 0.000000000000000000 ) ) ;
#7215 = DIRECTION ( 'NONE',  ( 0.000000000000000000, 0.000000000000000000, -1.000000000000000000 ) ) ;
#7216 = ORIENTED_EDGE ( 'NONE', *, *, #5528, .F. ) ;
#7217 = CARTESIAN_POINT ( 'NONE',  ( 609.8579287883226243, 189.7296425882048823, 189.8646579186752774 ) ) ;
#7218 = FACE_OUTER_BOUND ( 'NONE', #1037, .T. ) ;
#7219 = CARTESIAN_POINT ( 'NONE',  ( 726.1975094929946408, 167.5243180396263938, 150.0000000000013642 ) ) ;
#7220 = CARTESIAN_POINT ( 'NONE',  ( 8.673617379884035472E-16, 4.618802153517012954, -5.000000000000000000 ) ) ;
#7221 = ORIENTED_EDGE ( 'NONE', *, *, #7, .T. ) ;
#7222 = SURFACE_SIDE_STYLE ('',( #1823 ) ) ;
#7223 = DIRECTION ( 'NONE',  ( -0.000000000000000000, -0.000000000000000000, 1.000000000000000000 ) ) ;
#7224 = ORIENTED_EDGE ( 'NONE', *, *, #2833, .F. ) ;
#7225 = DIRECTION ( 'NONE',  ( 0.000000000000000000, 0.000000000000000000, -1.000000000000000000 ) ) ;
#7226 = ORIENTED_EDGE ( 'NONE', *, *, #13399, .F. ) ;
#7227 = ORIENTED_EDGE ( 'NONE', *, *, #9551, .F. ) ;
#7228 = CARTESIAN_POINT ( 'NONE',  ( 107.2182642636026202, 357.3942142120087055, 190.0000000000000000 ) ) ;
#7229 = DIRECTION ( 'NONE',  ( 0.000000000000000000, 1.000000000000000000, 3.264827003555234768E-15 ) ) ;
#7230 = CARTESIAN_POINT ( 'NONE',  ( 716.7018481736365629, 193.3416907550376322, 179.8000000000001535 ) ) ;
#7231 = CARTESIAN_POINT ( 'NONE',  ( 470.8287951810180516, 310.9528939902474463, 210.0000000000000000 ) ) ;
#7232 = PRODUCT_DEFINITION_CONTEXT ( 'detailed design', #13570, 'design' ) ;
#7233 = DIRECTION ( 'NONE',  ( -1.000000000000000000, 0.000000000000000000, 0.000000000000000000 ) ) ;
#7234 = EDGE_LOOP ( 'NONE', ( #14029, #12856, #10826 ) ) ;
#7235 = CYLINDRICAL_SURFACE ( 'NONE', #11274, 6.080745460913608902 ) ;
#7236 = FACE_BOUND ( 'NONE', #9929, .T. ) ;
#7237 = DIRECTION ( 'NONE',  ( 0.000000000000000000, 0.000000000000000000, 1.000000000000000000 ) ) ;
#7238 = AXIS2_PLACEMENT_3D ( 'NONE', #7753, #13287, #3111 ) ;
#7239 = VECTOR ( 'NONE', #10856, 1000.000000000000227 ) ;
#7240 = CARTESIAN_POINT ( 'NONE',  ( 0.000000000000000000, 0.000000000000000000, -8.000000000000000000 ) ) ;
#7241 = VECTOR ( 'NONE', #8084, 1000.000000000000000 ) ;
#7242 = VERTEX_POINT ( 'NONE', #3387 ) ;
#7243 = ORIENTED_EDGE ( 'NONE', *, *, #8996, .F. ) ;
#7244 = DIRECTION ( 'NONE',  ( 0.000000000000000000, 1.000000000000000000, 0.000000000000000000 ) ) ;
#7245 = DIRECTION ( 'NONE',  ( 2.022127743178574844E-16, 3.939404418192334771E-15, -1.000000000000000000 ) ) ;
#7246 = EDGE_CURVE ( 'NONE', #6340, #6556, #12441, .T. ) ;
#7247 = CARTESIAN_POINT ( 'NONE',  ( -5.450967621166011412, 4.358435876041001578, -0.3607371497494529233 ) ) ;
#7248 = CARTESIAN_POINT ( 'NONE',  ( 610.0000000000001137, 191.1080398579018720, -190.0000000000000000 ) ) ;
#7250 = ORIENTED_EDGE ( 'NONE', *, *, #1504, .F. ) ;
#7249 = AXIS2_PLACEMENT_3D ( 'NONE', #9367, #2878, #1609 ) ;
#7251 = AXIS2_PLACEMENT_3D ( 'NONE', #13043, #7426, #8825 ) ;
#7252 = DIRECTION ( 'NONE',  ( -1.000000000000000000, 0.000000000000000000, 0.000000000000000000 ) ) ;
#7253 = CARTESIAN_POINT ( 'NONE',  ( 6.506987859255521478, -2.925375531177301980, -5.066899051217866656 ) ) ;
#7254 = CARTESIAN_POINT ( 'NONE',  ( 2.999999999999999112, 2.309401076758508253, 3.999999999999993339 ) ) ;
#7255 = CARTESIAN_POINT ( 'NONE',  ( 2.500000000000000000, -1.178949249685214307, 2.042000000000001592 ) ) ;
#7256 = LINE ( 'NONE', #11744, #8666 ) ;
#7257 = LINE ( 'NONE', #1507, #1260 ) ;
#7258 =( REPRESENTATION_RELATIONSHIP ('NONE','NONE', #2822, #9337 ) REPRESENTATION_RELATIONSHIP_WITH_TRANSFORMATION ( #3155 )SHAPE_REPRESENTATION_RELATIONSHIP( ) );
#7259 = ORIENTED_EDGE ( 'NONE', *, *, #9910, .T. ) ;
#7260 = CARTESIAN_POINT ( 'NONE',  ( 2.500000000000000444, 0.000000000000000000, -5.000000000000000888 ) ) ;
#7261 = EDGE_LOOP ( 'NONE', ( #2103, #2578 ) ) ;
#7262 = ORIENTED_EDGE ( 'NONE', *, *, #13827, .F. ) ;
#7263 = CYLINDRICAL_SURFACE ( 'NONE', #2382, 2.649999999999985700 ) ;
#7264 = ADVANCED_FACE ( 'NONE', ( #12525 ), #9125, .T. ) ;
#7265 = CIRCLE ( 'NONE', #2549, 5.200000000000005507 ) ;
#7266 = DIRECTION ( 'NONE',  ( 1.000000000000000000, 0.000000000000000000, 0.000000000000000000 ) ) ;
#7267 = DIRECTION ( 'NONE',  ( 1.000000000000000000, 0.000000000000000000, 0.000000000000000000 ) ) ;
#7269 = EDGE_CURVE ( 'NONE', #2855, #808, #2374, .T. ) ;
#7268 = LINE ( 'NONE', #8225, #5368 ) ;
#7270 = ORIENTED_EDGE ( 'NONE', *, *, #3435, .F. ) ;
#7271 = LINE ( 'NONE', #9345, #9715 ) ;
#7272 = AXIS2_PLACEMENT_3D ( 'NONE', #7382, #6127, #11796 ) ;
#7273 = CARTESIAN_POINT ( 'NONE',  ( 636.7009106935324780, 155.5114698605638637, 211.0000000000000000 ) ) ;
#7274 = DIRECTION ( 'NONE',  ( 1.078061080328271264E-15, 7.457226491206363694E-15, 1.000000000000000000 ) ) ;
#7275 = VERTEX_POINT ( 'NONE', #2255 ) ;
#7276 = SURFACE_SIDE_STYLE ('',( #4860 ) ) ;
#7277 = CARTESIAN_POINT ( 'NONE',  ( 610.7405786874708156, 188.6041887390371130, 185.0905558487023370 ) ) ;
#7278 = VERTEX_POINT ( 'NONE', #4715 ) ;
#7279 = VECTOR ( 'NONE', #6859, 1000.000000000000000 ) ;
#7280 = CARTESIAN_POINT ( 'NONE',  ( 0.000000000000000000, 0.000000000000000000, -190.0000000000000000 ) ) ;
#7281 = CONICAL_SURFACE ( 'NONE', #6581, 2.054999999999999716, 0.7853981633974482790 ) ;
#7282 = CARTESIAN_POINT ( 'NONE',  ( -1.399999999999998579, 9.184850993605147944E-16, 7.500000000000000000 ) ) ;
#7283 = EDGE_CURVE ( 'NONE', #9217, #9854, #13628, .T. ) ;
#7284 = B_SPLINE_CURVE_WITH_KNOTS ( 'NONE', 3,
 ( #3944, #11539, #5126, #8431, #8140, #12647 ),
 .UNSPECIFIED., .F., .F.,
 ( 4, 2, 4 ),
 ( -3.640115492410698714E-06, 0.0002066546034003381217, 0.0004169493222930869755 ),
 .UNSPECIFIED. ) ;
#7285 = VERTEX_POINT ( 'NONE', #11346 ) ;
#7286 = CARTESIAN_POINT ( 'NONE',  ( 609.6829874266189790, 186.4320250235422805, 187.4339272673398398 ) ) ;
#7287 = AXIS2_PLACEMENT_3D ( 'NONE', #3092, #1980, #10979 ) ;
#7288 = EDGE_CURVE ( 'NONE', #4304, #3815, #11766, .T. ) ;
#7289 = FACE_OUTER_BOUND ( 'NONE', #3794, .T. ) ;
#7290 =( LENGTH_UNIT ( ) NAMED_UNIT ( * ) SI_UNIT ( .MILLI., .METRE. ) );
#7291 = CARTESIAN_POINT ( 'NONE',  ( -1.948734328186081425E-15, 7.693909156114108860, -6.460786012260014921 ) ) ;
#7292 = ORIENTED_EDGE ( 'NONE', *, *, #6301, .F. ) ;
#7293 = AXIS2_PLACEMENT_3D ( 'NONE', #5401, #13296, #11077 ) ;
#7294 = DIRECTION ( 'NONE',  ( 0.000000000000000000, 0.000000000000000000, 1.000000000000000000 ) ) ;
#7295 = DIRECTION ( 'NONE',  ( 0.000000000000000000, -0.8660254037844381525, -0.5000000000000009992 ) ) ;
#7296 = ORIENTED_EDGE ( 'NONE', *, *, #2629, .T. ) ;
#7297 = ORIENTED_EDGE ( 'NONE', *, *, #3876, .F. ) ;
#7298 = ORIENTED_EDGE ( 'NONE', *, *, #1976, .T. ) ;
#7299 = LINE ( 'NONE', #1828, #11734 ) ;
#7300 = CIRCLE ( 'NONE', #11068, 5.560781378645573980 ) ;
#7301 = CARTESIAN_POINT ( 'NONE',  ( 4.366061277241453098, -4.984806845751389659, -0.09463688534107157768 ) ) ;
#7303 = AXIS2_PLACEMENT_3D ( 'NONE', #14016, #8387, #14078 ) ;
#7302 = DIRECTION ( 'NONE',  ( -0.2873478855663454401, -0.9578262852211514300, 0.000000000000000000 ) ) ;
#7304 = AXIS2_PLACEMENT_3D ( 'NONE', #9502, #6094, #1452 ) ;
#7305 = LINE ( 'NONE', #7231, #10625 ) ;
#7306 = CIRCLE ( 'NONE', #933, 2.649999999999985700 ) ;
#7307 = DIRECTION ( 'NONE',  ( -0.9578262852211506528, 0.2873478855663477161, -0.000000000000000000 ) ) ;
#7308 = VERTEX_POINT ( 'NONE', #6843 ) ;
#7309 = DIRECTION ( 'NONE',  ( 0.000000000000000000, -0.000000000000000000, 1.000000000000000000 ) ) ;
#7310 = CARTESIAN_POINT ( 'NONE',  ( 0.3572655899081607078, 2.309401076758500704, -4.000000000000000000 ) ) ;
#7311 = CIRCLE ( 'NONE', #1426, 5.100000000000000533 ) ;
#7312 = CARTESIAN_POINT ( 'NONE',  ( 0.000000000000000000, -1.178949249685214307, 2.042000000000001592 ) ) ;
#7313 = ADVANCED_FACE ( 'NONE', ( #1306 ), #5803, .T. ) ;
#7314 = VECTOR ( 'NONE', #13091, 1000.000000000000000 ) ;
#7315 = EDGE_LOOP ( 'NONE', ( #11033, #9022, #8987, #12342 ) ) ;
#7316 = ORIENTED_EDGE ( 'NONE', *, *, #8403, .T. ) ;
#7317 = DIRECTION ( 'NONE',  ( 0.000000000000000000, 0.000000000000000000, -1.000000000000000000 ) ) ;
#7318 = DIRECTION ( 'NONE',  ( -0.9578262852211503198, 0.2873478855663487153, -1.489419751501257816E-15 ) ) ;
#7319 = EDGE_CURVE ( 'NONE', #11016, #8855, #13193, .T. ) ;
#7320 = PLANE ( 'NONE',  #7773 ) ;
#7321 = CIRCLE ( 'NONE', #9211, 4.199999999999926459 ) ;
#7322 = CIRCLE ( 'NONE', #10858, 4.199999999999981526 ) ;
#7323 = CARTESIAN_POINT ( 'NONE',  ( 21.00000000000000355, 0.000000000000000000, 0.000000000000000000 ) ) ;
#7324 = AXIS2_PLACEMENT_3D ( 'NONE', #7523, #4139, #861 ) ;
#7325 = ORIENTED_EDGE ( 'NONE', *, *, #12653, .F. ) ;
#7326 = MECHANICAL_DESIGN_GEOMETRIC_PRESENTATION_REPRESENTATION (  '', ( #3088 ), #953 ) ;
#7327 = DIRECTION ( 'NONE',  ( 0.000000000000000000, 1.224646799147353207E-16, 1.000000000000000000 ) ) ;
#7328 = PLANE ( 'NONE',  #14435 ) ;
#7329 = CARTESIAN_POINT ( 'NONE',  ( -2.000000000000007550, -3.464101615137749945, 0.000000000000000000 ) ) ;
#7330 = EDGE_CURVE ( 'NONE', #9114, #9269, #14352, .T. ) ;
#7331 = CARTESIAN_POINT ( 'NONE',  ( 635.0000000000000000, 160.0000000000000284, -210.0000000000000000 ) ) ;
#7332 = CARTESIAN_POINT ( 'NONE',  ( -6.837824896291515131, -3.947820044545435447, -6.564402953523717166 ) ) ;
#7333 = CARTESIAN_POINT ( 'NONE',  ( -3.510273485745307287, -2.827716139362669967, -3.610536846335890004 ) ) ;
#7334 =( NAMED_UNIT ( * ) SI_UNIT ( $, .STERADIAN. ) SOLID_ANGLE_UNIT ( ) );
#7335 = CIRCLE ( 'NONE', #13949, 0.7500000000000000000 ) ;
#7336 = ORIENTED_EDGE ( 'NONE', *, *, #11248, .F. ) ;
#7337 = AXIS2_PLACEMENT_3D ( 'NONE', #543, #9494, #14001 ) ;
#7338 = CARTESIAN_POINT ( 'NONE',  ( 3.455068668934414777, -2.624017327439094327, -3.316620875263732504 ) ) ;
#7339 = ORIENTED_EDGE ( 'NONE', *, *, #8485, .F. ) ;
#7340 = VERTEX_POINT ( 'NONE', #10387 ) ;
#7341 = DIRECTION ( 'NONE',  ( -0.2873478855663361697, -0.9578262852211543166, 0.000000000000000000 ) ) ;
#7342 = VECTOR ( 'NONE', #3083, 1000.000000000000000 ) ;
#7343 = CYLINDRICAL_SURFACE ( 'NONE', #4745, 4.799999999999968736 ) ;
#7344 = AXIS2_PLACEMENT_3D ( 'NONE', #1584, #10457, #11844 ) ;
#7345 = CARTESIAN_POINT ( 'NONE',  ( 610.0000000000000000, 0.000000000000000000, 190.0000000000000000 ) ) ;
#7346 = CARTESIAN_POINT ( 'NONE',  ( 451.6722694765949768, 316.6998517015743460, 210.0000000000000000 ) ) ;
#7347 = EDGE_LOOP ( 'NONE', ( #13768, #2013 ) ) ;
#7348 = PLANE ( 'NONE',  #3581 ) ;
#7349 = APPLICATION_CONTEXT ( 'automotive_design' ) ;
#7350 = EDGE_CURVE ( 'NONE', #10329, #12967, #11559, .T. ) ;
#7351 = CARTESIAN_POINT ( 'NONE',  ( -10.00000000000000000, -10.00000000000000000, -210.0000000000000000 ) ) ;
#7352 = MECHANICAL_DESIGN_GEOMETRIC_PRESENTATION_REPRESENTATION (  '', ( #6875 ), #6423 ) ;
#7353 = CARTESIAN_POINT ( 'NONE',  ( 142.4540310085880606, 355.9707293956415697, 187.0000000000000000 ) ) ;
#7354 = DIRECTION ( 'NONE',  ( 0.9578262852211507639, -0.2873478855663477716, 0.000000000000000000 ) ) ;
#7355 = ORIENTED_EDGE ( 'NONE', *, *, #11337, .F. ) ;
#7356 = CARTESIAN_POINT ( 'NONE',  ( 2.971071886220372438, 5.790204346174072647, 1.063026348804146728E-15 ) ) ;
#7357 = FACE_OUTER_BOUND ( 'NONE', #6680, .T. ) ;
#7358 = ORIENTED_EDGE ( 'NONE', *, *, #8452, .T. ) ;
#7359 = VECTOR ( 'NONE', #8167, 1000.000000000000000 ) ;
#7360 = FACE_OUTER_BOUND ( 'NONE', #9559, .T. ) ;
#7361 = PRODUCT_DEFINITION_SHAPE ( 'NONE', 'NONE',  #14625 ) ;
#7362 = PRODUCT_DEFINITION_FORMATION_WITH_SPECIFIED_SOURCE ( 'ANY', '', #2394, .NOT_KNOWN. ) ;
#7363 = CARTESIAN_POINT ( 'NONE',  ( 0.3572655899081652042, 4.618802153517012066, 5.829523438926728986E-16 ) ) ;
#7364 = DIRECTION ( 'NONE',  ( -1.000000000000000000, 0.000000000000000000, 0.000000000000000000 ) ) ;
#7365 = EDGE_CURVE ( 'NONE', #4582, #11448, #10996, .T. ) ;
#7366 =( GEOMETRIC_REPRESENTATION_CONTEXT ( 3 ) GLOBAL_UNCERTAINTY_ASSIGNED_CONTEXT ( ( #3561 ) ) GLOBAL_UNIT_ASSIGNED_CONTEXT ( ( #1076, #5874, #10236 ) ) REPRESENTATION_CONTEXT ( 'NONE', 'WORKASPACE' ) );
#7367 = VERTEX_POINT ( 'NONE', #5080 ) ;
#7368 = CARTESIAN_POINT ( 'NONE',  ( 610.6294623944595514, 188.6821150189054777, 185.3758453455904771 ) ) ;
#7369 = ADVANCED_FACE ( 'NONE', ( #11697, #8235, #10603, #5145, #10746, #7140 ), #11633, .F. ) ;
#7370 = CARTESIAN_POINT ( 'NONE',  ( 610.1557962250110450, 190.0426856094898085, -186.7771368031600048 ) ) ;
#7371 = LINE ( 'NONE', #9442, #4972 ) ;
#7372 = CARTESIAN_POINT ( 'NONE',  ( 0.000000000000000000, 3.306546357697853733E-16, -2.700000000000000178 ) ) ;
#7373 = ORIENTED_EDGE ( 'NONE', *, *, #6752, .F. ) ;
#7374 = PRODUCT ( 'Mirrorsliding track^MAS-180', 'Mirrorsliding track^MAS-180', '', ( #8793 ) ) ;
#7375 = DIRECTION ( 'NONE',  ( -0.2873478855663502141, -0.9578262852211498757, -4.782469237902382669E-30 ) ) ;
#7376 = CARTESIAN_POINT ( 'NONE',  ( 6.371506350351443082, 3.439339428956428968, -4.260454149911181432 ) ) ;
#7377 = ORIENTED_EDGE ( 'NONE', *, *, #8961, .T. ) ;
#7378 = ADVANCED_FACE ( 'NONE', ( #9648 ), #12889, .F. ) ;
#7379 = EDGE_CURVE ( 'NONE', #8163, #11431, #11767, .T. ) ;
#7380 = ORIENTED_EDGE ( 'NONE', *, *, #2609, .T. ) ;
#7381 = VECTOR ( 'NONE', #1057, 1000.000000000000114 ) ;
#7382 = CARTESIAN_POINT ( 'NONE',  ( 716.7018481736364492, 193.3416907550376322, 182.8000000000001535 ) ) ;
#7384 = ADVANCED_FACE ( 'NONE', ( #4930 ), #6355, .T. ) ;
#7383 = VECTOR ( 'NONE', #13989, 1000.000000000000000 ) ;
#7385 = DIRECTION ( 'NONE',  ( -1.000000000000000000, 0.000000000000000000, 0.000000000000000000 ) ) ;
#7386 = DIRECTION ( 'NONE',  ( 0.2873478855663466613, 0.9578262852211509859, 0.000000000000000000 ) ) ;
#7387 = CARTESIAN_POINT ( 'NONE',  ( 641.0000000000000000, 166.0000000000000284, -187.5000000000000000 ) ) ;
#7388 = UNCERTAINTY_MEASURE_WITH_UNIT (LENGTH_MEASURE( 1.000000000000000082E-05 ), #3883, 'distance_accuracy_value', 'NONE');
#7389 = CARTESIAN_POINT ( 'NONE',  ( 635.0000000000000000, 160.0000000000000284, -211.0000000000000000 ) ) ;
#7390 = VERTEX_POINT ( 'NONE', #12822 ) ;
#7391 = CLOSED_SHELL ( 'NONE', ( #11467, #1131, #5423, #5132, #11065, #812, #10520, #1870, #2041, #5039, #11432, #6250, #1933, #6841, #3948, #3035, #7744, #9761, #160, #11055, #12050, #1374, #5142, #3920, #9451, #11294, #1044, #9174, #12211, #807 ) ) ;
#7392 = CARTESIAN_POINT ( 'NONE',  ( 8.500000000000000000, 5.773502691896261751, 0.000000000000000000 ) ) ;
#7393 = B_SPLINE_CURVE_WITH_KNOTS ( 'NONE', 3,
 ( #14431, #8459, #5016, #11018, #1529, #9513 ),
 .UNSPECIFIED., .F., .F.,
 ( 4, 2, 4 ),
 ( 0.000000000000000000, 0.0002095117440864783663, 0.0004190234881729567326 ),
 .UNSPECIFIED. ) ;
#7394 = DIRECTION ( 'NONE',  ( 0.9578262852211517631, -0.2873478855663438858, 0.000000000000000000 ) ) ;
#7395 = DIRECTION ( 'NONE',  ( 0.000000000000000000, 0.000000000000000000, -1.000000000000000000 ) ) ;
#7396 = EDGE_CURVE ( 'NONE', #7275, #3159, #13656, .T. ) ;
#7397 = EDGE_CURVE ( 'NONE', #14524, #3289, #1591, .T. ) ;
#7398 = LINE ( 'NONE', #1926, #2608 ) ;
#7399 = ORIENTED_EDGE ( 'NONE', *, *, #12774, .F. ) ;
#7400 = ORIENTED_EDGE ( 'NONE', *, *, #4047, .F. ) ;
#7401 = FACE_OUTER_BOUND ( 'NONE', #10802, .T. ) ;
#7402 = LINE ( 'NONE', #13084, #2607 ) ;
#7403 = CARTESIAN_POINT ( 'NONE',  ( 635.0000000000000000, 160.0000000000000284, -187.5000000000000000 ) ) ;
#7404 = FACE_OUTER_BOUND ( 'NONE', #4742, .T. ) ;
#7405 = ORIENTED_EDGE ( 'NONE', *, *, #11928, .F. ) ;
#7406 = EDGE_CURVE ( 'NONE', #10624, #8163, #6103, .T. ) ;
#7407 = CARTESIAN_POINT ( 'NONE',  ( 641.0000000000000000, 154.0000000000000568, 187.5000000000000000 ) ) ;
#7408 = CARTESIAN_POINT ( 'NONE',  ( 5.727634848076855967, 4.575561887447700649, -6.326622577870477215 ) ) ;
#7409 = CARTESIAN_POINT ( 'NONE',  ( 0.000000000000000000, 0.000000000000000000, -5.000000000000000888 ) ) ;
#7410 = EDGE_CURVE ( 'NONE', #2268, #696, #10463, .T. ) ;
#7411 = CARTESIAN_POINT ( 'NONE',  ( 0.3572655899080433572, -2.309401076758680116, -4.000000000000000000 ) ) ;
#7412 = CARTESIAN_POINT ( 'NONE',  ( 610.8620436566989156, 230.3137853645742155, -190.0000000000000000 ) ) ;
#7413 = CARTESIAN_POINT ( 'NONE',  ( 610.0000000000000000, 227.4403065089105951, -190.0000000000000000 ) ) ;
#7414 = ORIENTED_EDGE ( 'NONE', *, *, #8258, .T. ) ;
#7415 = CARTESIAN_POINT ( 'NONE',  ( 0.000000000000000000, 5.258101095580073669E-15, 4.000000000000000000 ) ) ;
#7416 = ORIENTED_EDGE ( 'NONE', *, *, #11596, .T. ) ;
#7417 = ORIENTED_EDGE ( 'NONE', *, *, #4276, .F. ) ;
#7418 = CARTESIAN_POINT ( 'NONE',  ( 139.8040310085880833, 355.9707293956415697, 187.0000000000000000 ) ) ;
#7419 = DIRECTION ( 'NONE',  ( -1.000000000000000000, -6.938893903907222067E-15, 0.000000000000000000 ) ) ;
#7420 = DIRECTION ( 'NONE',  ( -1.000000000000000000, -0.000000000000000000, -0.000000000000000000 ) ) ;
#7421 = DIRECTION ( 'NONE',  ( 0.000000000000000000, 0.000000000000000000, -1.000000000000000000 ) ) ;
#7422 = MANIFOLD_SOLID_BREP ( 'Cut-Extrude1', #9280 ) ;
#7423 = ORIENTED_EDGE ( 'NONE', *, *, #11721, .F. ) ;
#7424 = DIRECTION ( 'NONE',  ( -1.000000000000000000, -0.000000000000000000, -0.000000000000000000 ) ) ;
#7425 = CARTESIAN_POINT ( 'NONE',  ( 6.826575449902429149, 2.663085462279306981, -6.347418139105299950 ) ) ;
#7426 = DIRECTION ( 'NONE',  ( -1.000000000000000000, -0.000000000000000000, -0.000000000000000000 ) ) ;
#7427 = CARTESIAN_POINT ( 'NONE',  ( 0.000000000000000000, 0.000000000000000000, -4.000000000000000000 ) ) ;
#7428 = ORIENTED_EDGE ( 'NONE', *, *, #13517, .F. ) ;
#7429 = DIRECTION ( 'NONE',  ( 1.000000000000000000, 2.312964634635740689E-15, 0.000000000000000000 ) ) ;
#7430 = ITEM_DEFINED_TRANSFORMATION ( 'NONE', 'NONE', #10908,  #9440 ) ;
#7431 = EDGE_LOOP ( 'NONE', ( #2095, #8649, #13672, #3630 ) ) ;
#7432 = EDGE_CURVE ( 'NONE', #3037, #1456, #2813, .T. ) ;
#7433 = CARTESIAN_POINT ( 'NONE',  ( -6.539196172010139030, 3.775406670193821146, -6.286444963328671420 ) ) ;
#7434 = FACE_OUTER_BOUND ( 'NONE', #9587, .T. ) ;
#7435 = ORIENTED_EDGE ( 'NONE', *, *, #5055, .F. ) ;
#7436 = CARTESIAN_POINT ( 'NONE',  ( 2.687328764639642653, -3.067272167851299969, -0.05923475698271395140 ) ) ;
#7437 = FACE_OUTER_BOUND ( 'NONE', #5335, .T. ) ;
#7438 = DIRECTION ( 'NONE',  ( 0.000000000000000000, 0.000000000000000000, 1.000000000000000000 ) ) ;
#7439 = VECTOR ( 'NONE', #9535, 1000.000000000000114 ) ;
#7440 = VERTEX_POINT ( 'NONE', #12138 ) ;
#7441 =( LENGTH_UNIT ( ) NAMED_UNIT ( * ) SI_UNIT ( .MILLI., .METRE. ) );
#7442 = CARTESIAN_POINT ( 'NONE',  ( 3.500000000000000000, 4.898587196589412829E-16, -4.000000000000000000 ) ) ;
#7443 = ORIENTED_EDGE ( 'NONE', *, *, #2229, .T. ) ;
#7444 = ORIENTED_EDGE ( 'NONE', *, *, #11652, .T. ) ;
#7445 = CARTESIAN_POINT ( 'NONE',  ( 2.500000000000000000, 0.000000000000000000, 0.000000000000000000 ) ) ;
#7446 = EDGE_CURVE ( 'NONE', #5805, #2398, #2556, .T. ) ;
#7447 = CYLINDRICAL_SURFACE ( 'NONE', #12468, 5.249999999999976907 ) ;
#7448 = EDGE_CURVE ( 'NONE', #3152, #10585, #5227, .T. ) ;
#7449 = CARTESIAN_POINT ( 'NONE',  ( 6.357976367242160975, 3.426708043488479127, -4.282301071215555588 ) ) ;
#7450 = DIRECTION ( 'NONE',  ( 1.000000000000000000, 0.000000000000000000, 0.000000000000000000 ) ) ;
#7451 = EDGE_CURVE ( 'NONE', #5548, #6439, #12226, .T. ) ;
#7452 = DIRECTION ( 'NONE',  ( -0.9237280213470676626, -0.3830490080632388272, 0.000000000000000000 ) ) ;
#7453 = ORIENTED_EDGE ( 'NONE', *, *, #10891, .F. ) ;
#7454 = EDGE_CURVE ( 'NONE', #14292, #30, #5876, .T. ) ;
#7455 = DIRECTION ( 'NONE',  ( 0.000000000000000000, 1.000000000000000000, -1.287488025362403787E-15 ) ) ;
#7456 = DIRECTION ( 'NONE',  ( -0.000000000000000000, 0.000000000000000000, 1.000000000000000000 ) ) ;
#7457 = DIRECTION ( 'NONE',  ( 0.000000000000000000, 1.000000000000000000, 0.000000000000000000 ) ) ;
#7458 = ORIENTED_EDGE ( 'NONE', *, *, #6365, .T. ) ;
#7459 = VERTEX_POINT ( 'NONE', #13393 ) ;
#7460 = FACE_OUTER_BOUND ( 'NONE', #13112, .T. ) ;
#7461 = PLANE ( 'NONE',  #7076 ) ;
#7462 = MANIFOLD_SOLID_BREP ( 'Boss-Extrude2', #2439 ) ;
#7463 = CARTESIAN_POINT ( 'NONE',  ( 609.7645211877446627, 186.0291131959509698, -186.4810828243464016 ) ) ;
#7464 = CARTESIAN_POINT ( 'NONE',  ( -1.500000000000001332, 0.000000000000000000, 0.000000000000000000 ) ) ;
#7465 = EDGE_CURVE ( 'NONE', #13301, #696, #12200, .T. ) ;
#7466 = ORIENTED_EDGE ( 'NONE', *, *, #1115, .F. ) ;
#7467 = ADVANCED_FACE ( 'NONE', ( #4118 ), #8763, .F. ) ;
#7468 = CARTESIAN_POINT ( 'NONE',  ( 7.336184427528458230, 0.000000000000000000, -8.105212085995399107 ) ) ;
#7469 = CARTESIAN_POINT ( 'NONE',  ( 10.00000000000000000, -9.999999999999998224, -190.0000000000000000 ) ) ;
#7470 = DIRECTION ( 'NONE',  ( -0.000000000000000000, -0.000000000000000000, -1.000000000000000000 ) ) ;
#7471 = ORIENTED_EDGE ( 'NONE', *, *, #12248, .T. ) ;
#7472 = EDGE_CURVE ( 'NONE', #5092, #7639, #2106, .T. ) ;
#7473 = VECTOR ( 'NONE', #3607, 1000.000000000000000 ) ;
#7474 = LINE ( 'NONE', #7255, #1118 ) ;
#7475 = DIRECTION ( 'NONE',  ( -1.000000000000000000, -7.930164461608254918E-15, 0.000000000000000000 ) ) ;
#7476 = LINE ( 'NONE', #2915, #1613 ) ;
#7477 =( NAMED_UNIT ( * ) SI_UNIT ( $, .STERADIAN. ) SOLID_ANGLE_UNIT ( ) );
#7478 = ORIENTED_EDGE ( 'NONE', *, *, #2363, .F. ) ;
#7479 = DIRECTION ( 'NONE',  ( 0.000000000000000000, 0.5000000000000009992, -0.8660254037844380415 ) ) ;
#7480 = EDGE_LOOP ( 'NONE', ( #2275, #7596, #2984, #3038 ) ) ;
#7481 = ORIENTED_EDGE ( 'NONE', *, *, #13985, .F. ) ;
#7482 = DIRECTION ( 'NONE',  ( 0.000000000000000000, 0.000000000000000000, 1.000000000000000000 ) ) ;
#7483 = CARTESIAN_POINT ( 'NONE',  ( 0.000000000000000000, 0.000000000000000000, 0.000000000000000000 ) ) ;
#7484 = AXIS2_PLACEMENT_3D ( 'NONE', #11693, #11555, #11763 ) ;
#7485 = VERTEX_POINT ( 'NONE', #13695 ) ;
#7486 = VECTOR ( 'NONE', #4668, 1000.000000000000000 ) ;
#7487 = ORIENTED_EDGE ( 'NONE', *, *, #12686, .F. ) ;
#7488 = DIRECTION ( 'NONE',  ( 0.000000000000000000, -1.000000000000000000, 0.000000000000000000 ) ) ;
#7489 = CARTESIAN_POINT ( 'NONE',  ( 634.0182522957533138, 167.5000000000000568, 210.0000119999999981 ) ) ;
#7490 = DIRECTION ( 'NONE',  ( -0.000000000000000000, -0.000000000000000000, 1.000000000000000000 ) ) ;
#7491 = DIRECTION ( 'NONE',  ( 0.000000000000000000, 0.000000000000000000, 1.000000000000000000 ) ) ;
#7492 = ORIENTED_EDGE ( 'NONE', *, *, #5299, .F. ) ;
#7493 = AXIS2_PLACEMENT_3D ( 'NONE', #6789, #5693, #8718 ) ;
#7494 = CARTESIAN_POINT ( 'NONE',  ( 609.7124105659718225, 187.8865375995820557, 188.9268648956065419 ) ) ;
#7495 = CARTESIAN_POINT ( 'NONE',  ( 641.0000000000000000, 154.0000000000000568, -187.5000000000000000 ) ) ;
#7496 = AXIS2_PLACEMENT_3D ( 'NONE', #11896, #14204, #10796 ) ;
#7497 = ORIENTED_EDGE ( 'NONE', *, *, #8850, .F. ) ;
#7498 = AXIS2_PLACEMENT_3D ( 'NONE', #12382, #1089, #10250 ) ;
#7499 = DIRECTION ( 'NONE',  ( -1.000000000000000000, 0.000000000000000000, 0.000000000000000000 ) ) ;
#7500 = VERTEX_POINT ( 'NONE', #2397 ) ;
#7501 = CARTESIAN_POINT ( 'NONE',  ( 590.0000000000000000, -9.999999999999941380, 190.0000000000000000 ) ) ;
#7502 = LINE ( 'NONE', #1896, #9230 ) ;
#7503 = VECTOR ( 'NONE', #6984, 1000.000000000000000 ) ;
#7504 = CIRCLE ( 'NONE', #9396, 0.1000000000000002554 ) ;
#7505 = AXIS2_PLACEMENT_3D ( 'NONE', #4756, #9244, #9091 ) ;
#7506 = VERTEX_POINT ( 'NONE', #11183 ) ;
#7507 = CARTESIAN_POINT ( 'NONE',  ( 610.0858458365329398, 190.4893660822393144, 186.9132285165672727 ) ) ;
#7508 = DIRECTION ( 'NONE',  ( 0.000000000000000000, 0.000000000000000000, 1.000000000000000000 ) ) ;
#7509 = DIRECTION ( 'NONE',  ( -0.000000000000000000, 1.000000000000000000, 1.224646799147353207E-16 ) ) ;
#7510 = ADVANCED_FACE ( 'NONE', ( #2240 ), #1356, .T. ) ;
#7511 = ORIENTED_EDGE ( 'NONE', *, *, #12792, .T. ) ;
#7513 = EDGE_CURVE ( 'NONE', #6803, #542, #10224, .T. ) ;
#7512 = DIRECTION ( 'NONE',  ( 1.000000000000000000, 0.000000000000000000, -0.000000000000000000 ) ) ;
#7514 = FILL_AREA_STYLE_COLOUR ( '', #14551 ) ;
#7515 = EDGE_LOOP ( 'NONE', ( #7400, #4256, #14109, #6031 ) ) ;
#7516 = AXIS2_PLACEMENT_3D ( 'NONE', #2079, #9098, #1114 ) ;
#7517 = VECTOR ( 'NONE', #2858, 1000.000000000000000 ) ;
#7518 = ORIENTED_EDGE ( 'NONE', *, *, #9547, .F. ) ;
#7519 = FACE_OUTER_BOUND ( 'NONE', #3720, .T. ) ;
#7520 =( BOUNDED_SURFACE ( )  B_SPLINE_SURFACE ( 3, 2, ( 
 ( #219, #3650, #8129 ),
 ( #12637, #2519, #1422 ),
 ( #296, #4832, #9324 ),
 ( #3718, #8201, #10939 ),
 ( #9829, #8579, #4090 ),
 ( #4223, #14331, #10786 ) ),
 .UNSPECIFIED., .F., .F., .T. ) 
 B_SPLINE_SURFACE_WITH_KNOTS ( ( 4, 2, 4 ),
 ( 3, 3 ),
 ( 0.02367865728600889244, 0.02663179453327095547, 0.02958493178053301503 ),
 ( 0.000000000000000000, 1.000000000000000000 ),
 .UNSPECIFIED. ) 
 GEOMETRIC_REPRESENTATION_ITEM ( )  RATIONAL_B_SPLINE_SURFACE ( (
 ( 1.000000000000000000, 0.8047781103519378032, 1.000000000000000000),
 ( 1.000000000000000000, 0.8123785825977077879, 1.000000000000000000),
 ( 1.000000000000000000, 0.8190671539292031511, 1.000000000000000000),
 ( 1.000000000000000000, 0.8192352255331103450, 1.000000000000000000),
 ( 1.000000000000000000, 0.8126129676838903526, 1.000000000000000000),
 ( 1.000000000000000000, 0.8047712537969723412, 1.000000000000000000) ) ) 
 REPRESENTATION_ITEM ( '' )  SURFACE ( )  );
#7521 = FACE_BOUND ( 'NONE', #3298, .T. ) ;
#7522 = MECHANICAL_DESIGN_GEOMETRIC_PRESENTATION_REPRESENTATION (  '', ( #11995 ), #4231 ) ;
#7523 = CARTESIAN_POINT ( 'NONE',  ( 101.4713065522755215, 338.2376885075850623, 1.342499394901007523E-12 ) ) ;
#7524 = FACE_OUTER_BOUND ( 'NONE', #50, .T. ) ;
#7525 = VECTOR ( 'NONE', #1402, 1000.000000000000000 ) ;
#7526 = VECTOR ( 'NONE', #12517, 1000.000000000000000 ) ;
#7527 = UNCERTAINTY_MEASURE_WITH_UNIT (LENGTH_MEASURE( 1.000000000000000082E-05 ), #13846, 'distance_accuracy_value', 'NONE');
#7528 = CARTESIAN_POINT ( 'NONE',  ( 0.000000000000000000, 4.618802153517012954, 6.505213034913018715E-16 ) ) ;
#7529 = ADVANCED_FACE ( 'NONE', ( #8077 ), #3287, .T. ) ;
#7530 = EDGE_LOOP ( 'NONE', ( #4334, #7065, #11157, #9568 ) ) ;
#7531 = DIRECTION ( 'NONE',  ( -0.000000000000000000, -0.000000000000000000, 1.000000000000000000 ) ) ;
#7532 = LINE ( 'NONE', #6435, #8938 ) ;
#7533 = APPLICATION_PROTOCOL_DEFINITION ( 'draft international standard', 'automotive_design', 1998, #10077 ) ;
#7534 = AXIS2_PLACEMENT_3D ( 'NONE', #4258, #13262, #10902 ) ;
#7535 = DIRECTION ( 'NONE',  ( 0.000000000000000000, 0.000000000000000000, 1.000000000000000000 ) ) ;
#7536 = VERTEX_POINT ( 'NONE', #12583 ) ;
#7537 = ORIENTED_EDGE ( 'NONE', *, *, #3048, .F. ) ;
#7538 = DIRECTION ( 'NONE',  ( 0.000000000000000000, 0.000000000000000000, 1.000000000000000000 ) ) ;
#7539 = CARTESIAN_POINT ( 'NONE',  ( 635.0000000000000000, 160.0000000000000284, 211.0000000000000000 ) ) ;
#7540 = CIRCLE ( 'NONE', #14378, 3.999999999999999112 ) ;
#7541 = EDGE_CURVE ( 'NONE', #11118, #1544, #3302, .T. ) ;
#7542 = AXIS2_PLACEMENT_3D ( 'NONE', #8149, #13930, #12739 ) ;
#7543 = CARTESIAN_POINT ( 'NONE',  ( 144.7991633467111683, 386.6211705227183870, -190.0000000000000568 ) ) ;
#7544 = APPLICATION_CONTEXT ( 'automotive_design' ) ;
#7545 = AXIS2_PLACEMENT_3D ( 'NONE', #8816, #3202, #7641 ) ;
#7546 = CARTESIAN_POINT ( 'NONE',  ( -1.269541193505925744E-15, 7.895640089090863789, -6.564402953523717166 ) ) ;
#7547 = AXIS2_PLACEMENT_3D ( 'NONE', #3594, #7795, #13546 ) ;
#7548 = ORIENTED_EDGE ( 'NONE', *, *, #5185, .F. ) ;
#7549 = CARTESIAN_POINT ( 'NONE',  ( 440.1783540539412343, 278.3868002927283101, 190.0000000000000000 ) ) ;
#7550 = EDGE_CURVE ( 'NONE', #14303, #7561, #4779, .T. ) ;
#7551 = VERTEX_POINT ( 'NONE', #13612 ) ;
#7552 = VECTOR ( 'NONE', #381, 1000.000000000000000 ) ;
#7553 =( GEOMETRIC_REPRESENTATION_CONTEXT ( 3 ) GLOBAL_UNCERTAINTY_ASSIGNED_CONTEXT ( ( #7847 ) ) GLOBAL_UNIT_ASSIGNED_CONTEXT ( ( #7290, #14086, #634 ) ) REPRESENTATION_CONTEXT ( 'NONE', 'WORKASPACE' ) );
#7554 = CARTESIAN_POINT ( 'NONE',  ( 5.200000000000002842, 0.000000000000000000, 0.000000000000000000 ) ) ;
#7555 = LINE ( 'NONE', #13160, #2081 ) ;
#7556 = DIRECTION ( 'NONE',  ( -1.000000000000000000, 0.000000000000000000, 0.000000000000000000 ) ) ;
#7557 = DIRECTION ( 'NONE',  ( 0.000000000000000000, 0.000000000000000000, 1.000000000000000000 ) ) ;
#7558 = ORIENTED_EDGE ( 'NONE', *, *, #853, .T. ) ;
#7559 = FACE_OUTER_BOUND ( 'NONE', #569, .T. ) ;
#7560 = ORIENTED_EDGE ( 'NONE', *, *, #13251, .T. ) ;
#7561 = VERTEX_POINT ( 'NONE', #5642 ) ;
#7562 = AXIS2_PLACEMENT_3D ( 'NONE', #11732, #13896, #361 ) ;
#7563 = EDGE_CURVE ( 'NONE', #4046, #2298, #13477, .T. ) ;
#7564 = DIRECTION ( 'NONE',  ( 9.794481010665704304E-16, 3.264827003555233190E-15, 1.000000000000000000 ) ) ;
#7565 = EDGE_CURVE ( 'NONE', #14237, #6201, #5789, .T. ) ;
#7566 = VECTOR ( 'NONE', #14465, 1000.000000000000114 ) ;
#7567 = EDGE_CURVE ( 'NONE', #6440, #12655, #14149, .T. ) ;
#7568 = DIRECTION ( 'NONE',  ( 0.000000000000000000, 0.000000000000000000, -1.000000000000000000 ) ) ;
#7569 = ORIENTED_EDGE ( 'NONE', *, *, #14433, .F. ) ;
#7570 = VECTOR ( 'NONE', #3105, 1000.000000000000000 ) ;
#7571 = ORIENTED_EDGE ( 'NONE', *, *, #1335, .F. ) ;
#7572 = DIRECTION ( 'NONE',  ( 0.000000000000000000, 0.000000000000000000, -1.000000000000000000 ) ) ;
#7573 = DIRECTION ( 'NONE',  ( 1.019665600948283644E-15, 3.398885336494278419E-15, -1.000000000000000000 ) ) ;
#7574 = VECTOR ( 'NONE', #3216, 1000.000000000000227 ) ;
#7575 = CARTESIAN_POINT ( 'NONE',  ( 0.1756481739660539498, -4.720212674038995360, -3.469390959564070620 ) ) ;
#7576 = CARTESIAN_POINT ( 'NONE',  ( -1.250000000000000000, -6.429618962271402616, -1.000000000000000000 ) ) ;
#7577 = ORIENTED_EDGE ( 'NONE', *, *, #7821, .F. ) ;
#7578 = AXIS2_PLACEMENT_3D ( 'NONE', #4123, #2867, #11860 ) ;
#7579 = CARTESIAN_POINT ( 'NONE',  ( 609.8848581100098727, 185.7487647174620520, 185.4822770966949008 ) ) ;
#7580 = CARTESIAN_POINT ( 'NONE',  ( 635.0000000000000000, 160.0000000000000284, 210.0000119999999981 ) ) ;
#7581 = EDGE_LOOP ( 'NONE', ( #9452, #11538, #4693, #8624 ) ) ;
#7582 = DIRECTION ( 'NONE',  ( 0.000000000000000000, 0.000000000000000000, -1.000000000000000000 ) ) ;
#7583 = EDGE_LOOP ( 'NONE', ( #9968, #7600, #11232, #3697 ) ) ;
#7584 = B_SPLINE_CURVE_WITH_KNOTS ( 'NONE', 3,
 ( #7363, #13054, #11857, #1749 ),
 .UNSPECIFIED., .F., .F.,
 ( 4, 4 ),
 ( 2.380737581619760596E-07, 0.002336974151641558160 ),
 .UNSPECIFIED. ) ;
#7585 = VECTOR ( 'NONE', #10183, 1000.000000000000114 ) ;
#7586 = DIRECTION ( 'NONE',  ( -0.000000000000000000, -0.000000000000000000, 1.000000000000000000 ) ) ;
#7587 = CARTESIAN_POINT ( 'NONE',  ( -0.5590169943749470072, 7.041719095097280880E-16, 5.750000000000000000 ) ) ;
#7588 =( GEOMETRIC_REPRESENTATION_CONTEXT ( 3 ) GLOBAL_UNCERTAINTY_ASSIGNED_CONTEXT ( ( #11939 ) ) GLOBAL_UNIT_ASSIGNED_CONTEXT ( ( #4163, #1109, #7916 ) ) REPRESENTATION_CONTEXT ( 'NONE', 'WORKASPACE' ) );
#7589 = ORIENTED_EDGE ( 'NONE', *, *, #11515, .F. ) ;
#7590 = CARTESIAN_POINT ( 'NONE',  ( 610.8707502976318438, 188.5815814653741427, 184.8000000000000682 ) ) ;
#7591 = DIRECTION ( 'NONE',  ( 1.000000000000000000, 0.000000000000000000, 0.000000000000000000 ) ) ;
#7592 = EDGE_CURVE ( 'NONE', #8855, #11016, #208, .T. ) ;
#7593 = CARTESIAN_POINT ( 'NONE',  ( 153.1991633467111456, 386.6211705227183870, 210.0000000000000000 ) ) ;
#7594 = FILL_AREA_STYLE_COLOUR ( '', #13210 ) ;
#7595 = VECTOR ( 'NONE', #5216, 1000.000000000000000 ) ;
#7596 = ORIENTED_EDGE ( 'NONE', *, *, #14437, .T. ) ;
#7597 = ADVANCED_FACE ( 'NONE', ( #7872 ), #12421, .F. ) ;
#7598 = DIRECTION ( 'NONE',  ( -0.2873478855663453846, -0.9578262852211513190, -0.000000000000000000 ) ) ;
#7599 = CARTESIAN_POINT ( 'NONE',  ( 3.399999999999999911, 0.000000000000000000, -0.4201245229258211977 ) ) ;
#7600 = ORIENTED_EDGE ( 'NONE', *, *, #7513, .F. ) ;
#7601 = CIRCLE ( 'NONE', #5674, 6.500000000000000888 ) ;
#7602 = ORIENTED_EDGE ( 'NONE', *, *, #4135, .T. ) ;
#7603 = DIRECTION ( 'NONE',  ( -0.000000000000000000, -0.000000000000000000, -1.000000000000000000 ) ) ;
#7604 = DIRECTION ( 'NONE',  ( 0.2873478855663454401, 0.9578262852211514300, -3.927332483172771155E-15 ) ) ;
#7605 = CIRCLE ( 'NONE', #3126, 2.500000000000000444 ) ;
#7606 = DIRECTION ( 'NONE',  ( -1.000000000000000000, -0.000000000000000000, -0.000000000000000000 ) ) ;
#7607 = ADVANCED_FACE ( 'NONE', ( #11249 ), #8001, .T. ) ;
#7608 = PRODUCT_DEFINITION_SHAPE ( 'NONE', 'NONE',  #8184 ) ;
#7609 = CARTESIAN_POINT ( 'NONE',  ( 3.500000000000000000, 0.000000000000000000, -2.700000000000000622 ) ) ;
#7610 = VERTEX_POINT ( 'NONE', #2652 ) ;
#7611 = DIRECTION ( 'NONE',  ( 1.000000000000000000, 0.000000000000000000, -0.000000000000000000 ) ) ;
#7612 = ORIENTED_EDGE ( 'NONE', *, *, #7410, .F. ) ;
#7613 = LINE ( 'NONE', #13075, #9124 ) ;
#7614 = CARTESIAN_POINT ( 'NONE',  ( 6.371506350351448411, -5.409331239960140536, -0.8483282427581464447 ) ) ;
#7615 = CARTESIAN_POINT ( 'NONE',  ( 455.5035746174796145, 294.6698471414878782, -218.0000000000000000 ) ) ;
#7616 = AXIS2_PLACEMENT_3D ( 'NONE', #6915, #11474, #1369 ) ;
#7618 = VECTOR ( 'NONE', #13156, 1000.000000000000114 ) ;
#7617 = DIRECTION ( 'NONE',  ( 9.794481010665704304E-16, 3.264827003555233190E-15, 1.000000000000000000 ) ) ;
#7619 =( BOUNDED_SURFACE ( )  B_SPLINE_SURFACE ( 3, 2, ( 
 ( #12190, #7782, #11390 ),
 ( #10635, #9032, #12572 ),
 ( #1280, #10552, #12845 ),
 ( #5778, #4682, #9175 ),
 ( #5631, #13464, #6889 ),
 ( #513, #6047, #11720 ) ),
 .UNSPECIFIED., .F., .F., .F. ) 
 B_SPLINE_SURFACE_WITH_KNOTS ( ( 4, 2, 4 ),
 ( 3, 3 ),
 ( 0.02027065861071770947, 0.02273072267836921331, 0.02519078674602071716 ),
 ( 0.000000000000000000, 1.000000000000000000 ),
 .UNSPECIFIED. ) 
 GEOMETRIC_REPRESENTATION_ITEM ( )  RATIONAL_B_SPLINE_SURFACE ( (
 ( 1.000000000000000000, 0.8047781708337304885, 1.000000000000000000),
 ( 1.000000000000000000, 0.8123765190705307671, 1.000000000000000000),
 ( 1.000000000000000000, 0.8190656277163975707, 1.000000000000000000),
 ( 1.000000000000000000, 0.8192366903512159348, 1.000000000000000000),
 ( 1.000000000000000000, 0.8126138454302893610, 1.000000000000000000),
 ( 1.000000000000000000, 0.8047712246031417660, 1.000000000000000000) ) ) 
 REPRESENTATION_ITEM ( '' )  SURFACE ( )  );
#7620 = VERTEX_POINT ( 'NONE', #11326 ) ;
#7621 = ADVANCED_FACE ( 'NONE', ( #9267 ), #152, .T. ) ;
#7622 = EDGE_LOOP ( 'NONE', ( #7336, #4914, #9536, #657 ) ) ;
#7623 = FILL_AREA_STYLE_COLOUR ( '', #1360 ) ;
#7624 = DIRECTION ( 'NONE',  ( -0.9578262852211513190, 0.2873478855663453846, 0.000000000000000000 ) ) ;
#7625 = CARTESIAN_POINT ( 'NONE',  ( 610.0000000000001137, 185.6790804732684705, -184.8000000000000398 ) ) ;
#7626 = ADVANCED_FACE ( 'NONE', ( #4695 ), #3548, .T. ) ;
#7627 = ADVANCED_FACE ( 'NONE', ( #6969 ), #12127, .F. ) ;
#7628 = DIRECTION ( 'NONE',  ( 0.000000000000000000, 1.224646799147343593E-16, 1.000000000000000000 ) ) ;
#7629 = ORIENTED_EDGE ( 'NONE', *, *, #11574, .T. ) ;
#7630 = CLOSED_SHELL ( 'NONE', ( #5559, #7829, #1191, #1636, #13066, #12893, #14164, #4560, #12019, #10204, #7019, #8664, #11170, #7059, #5373, #11867, #13319, #6751, #1151, #3676, #6322, #12681, #8395, #9992, #2381, #3701, #13964 ) ) ;
#7631 = CARTESIAN_POINT ( 'NONE',  ( -20.63749999999999574, 0.000000000000000000, -6.750000000000000000 ) ) ;
#7632 = ORIENTED_EDGE ( 'NONE', *, *, #2697, .F. ) ;
#7633 = CARTESIAN_POINT ( 'NONE',  ( 707.5067158355133188, 162.6912496279604738, 177.6000000000001648 ) ) ;
#7634 = CARTESIAN_POINT ( 'NONE',  ( -5.699988423468465015, -4.591578518468254266, -6.344710093416085606 ) ) ;
#7635 = CYLINDRICAL_SURFACE ( 'NONE', #2548, 2.199999999999984635 ) ;
#7636 = SURFACE_STYLE_USAGE ( .BOTH. , #3133 ) ;
#7637 = ORIENTED_EDGE ( 'NONE', *, *, #10461, .F. ) ;
#7638 = CARTESIAN_POINT ( 'NONE',  ( 1.250000000000000000, -6.429618962271402616, -1.000000000000000000 ) ) ;
#7639 = VERTEX_POINT ( 'NONE', #3731 ) ;
#7640 = ORIENTED_EDGE ( 'NONE', *, *, #11246, .T. ) ;
#7641 = DIRECTION ( 'NONE',  ( -1.000000000000000000, 0.000000000000000000, 0.000000000000000000 ) ) ;
#7642 = CARTESIAN_POINT ( 'NONE',  ( 0.000000000000000000, 0.000000000000000000, -8.000000000000000000 ) ) ;
#7643 = ADVANCED_FACE ( 'NONE', ( #7038 ), #3814, .T. ) ;
#7644 = CARTESIAN_POINT ( 'NONE',  ( -3.355112389629170799, 2.681727112203152963, -0.2256878752776689534 ) ) ;
#7645 = EDGE_CURVE ( 'NONE', #4981, #10556, #7300, .T. ) ;
#7646 = ORIENTED_EDGE ( 'NONE', *, *, #10275, .T. ) ;
#7647 = ORIENTED_EDGE ( 'NONE', *, *, #13827, .T. ) ;
#7648 = CARTESIAN_POINT ( 'NONE',  ( 6.327632967269667397, -5.346704644972363418, 0.7392359018475850307 ) ) ;
#7649 = CARTESIAN_POINT ( 'NONE',  ( 627.5000000000000000, 160.0000000000000284, 210.0000059999999849 ) ) ;
#7650 = ADVANCED_FACE ( 'NONE', ( #6008 ), #5187, .T. ) ;
#7651 = CARTESIAN_POINT ( 'NONE',  ( -1.257172072275743346, 3.892973519171203378, -3.433252694550776862 ) ) ;
#7652 = CARTESIAN_POINT ( 'NONE',  ( -0.6810597143197697489, -4.461075778259609770, -3.598441714920717516 ) ) ;
#7653 = LINE ( 'NONE', #8826, #13046 ) ;
#7654 = ORIENTED_EDGE ( 'NONE', *, *, #12631, .F. ) ;
#7655 = EDGE_CURVE ( 'NONE', #2544, #13374, #13433, .T. ) ;
#7656 = CARTESIAN_POINT ( 'NONE',  ( 609.7152679600854981, 186.3148376777868975, 187.1062553063055418 ) ) ;
#7657 = CONTEXT_DEPENDENT_SHAPE_REPRESENTATION ( #6312, #14208 ) ;
#7658 = VERTEX_POINT ( 'NONE', #1571 ) ;
#7659 = CARTESIAN_POINT ( 'NONE',  ( 604.3113219698371950, -181.2933965909544725, 150.0000000000013358 ) ) ;
#7660 = ORIENTED_EDGE ( 'NONE', *, *, #5219, .T. ) ;
#7661 = CARTESIAN_POINT ( 'NONE',  ( -7.882332067283284779E-16, -3.838309248099061932, -3.351853367130940509 ) ) ;
#7662 = DIRECTION ( 'NONE',  ( -0.000000000000000000, -0.000000000000000000, -1.000000000000000000 ) ) ;
#7663 = ORIENTED_EDGE ( 'NONE', *, *, #11675, .F. ) ;
#7664 = CARTESIAN_POINT ( 'NONE',  ( 635.0000000000000000, 160.0000000000000284, 187.5000000000000000 ) ) ;
#7665 = DIRECTION ( 'NONE',  ( -0.000000000000000000, -0.000000000000000000, 1.000000000000000000 ) ) ;
#7666 = EDGE_CURVE ( 'NONE', #2593, #9335, #2535, .T. ) ;
#7667 = EDGE_CURVE ( 'NONE', #11448, #8086, #1304, .T. ) ;
#7668 = CARTESIAN_POINT ( 'NONE',  ( 3.700000000000000178, 0.000000000000000000, 0.000000000000000000 ) ) ;
#7669 = ORIENTED_EDGE ( 'NONE', *, *, #4932, .F. ) ;
#7670 = EDGE_CURVE ( 'NONE', #4684, #1652, #7123, .T. ) ;
#7671 = SURFACE_SIDE_STYLE ('',( #13124 ) ) ;
#7672 = ORIENTED_EDGE ( 'NONE', *, *, #11012, .F. ) ;
#7673 = AXIS2_PLACEMENT_3D ( 'NONE', #6350, #13138, #8709 ) ;
#7674 = VERTEX_POINT ( 'NONE', #7260 ) ;
#7675 = CARTESIAN_POINT ( 'NONE',  ( 1.098735407079012738, -7.248058225758961193, -6.326622577870306685 ) ) ;
#7676 = CARTESIAN_POINT ( 'NONE',  ( 630.3995367089856927, 153.9937209916067786, -210.0000000000000000 ) ) ;
#7677 = CARTESIAN_POINT ( 'NONE',  ( -0.2500000000000000000, -8.096141056083446585, -1.000000000000000000 ) ) ;
#7678 = VECTOR ( 'NONE', #11589, 1000.000000000000114 ) ;
#7679 = DIRECTION ( 'NONE',  ( 0.000000000000000000, 0.000000000000000000, -1.000000000000000000 ) ) ;
#7680 = FACE_OUTER_BOUND ( 'NONE', #10261, .T. ) ;
#7681 = EDGE_LOOP ( 'NONE', ( #13753, #7211 ) ) ;
#7682 = DIRECTION ( 'NONE',  ( -0.5000000000000051070, 1.060575238724903217E-16, -0.8660254037844355990 ) ) ;
#7683 = DIRECTION ( 'NONE',  ( 0.000000000000000000, 0.000000000000000000, 1.000000000000000000 ) ) ;
#7684 = ITEM_DEFINED_TRANSFORMATION ( 'NONE', 'NONE', #10897,  #9440 ) ;
#7685 = DIRECTION ( 'NONE',  ( 0.000000000000000000, 0.000000000000000000, 1.000000000000000000 ) ) ;
#7686 = ORIENTED_EDGE ( 'NONE', *, *, #6202, .T. ) ;
#7687 = VERTEX_POINT ( 'NONE', #375 ) ;
#7688 = FILL_AREA_STYLE ('',( #7623 ) ) ;
#7689 = CARTESIAN_POINT ( 'NONE',  ( -3.809068165403726614, -5.306386968807666804, -4.619717694324952472E-15 ) ) ;
#7690 = CARTESIAN_POINT ( 'NONE',  ( -8.074769166705394241, 378.0965165842501392, 187.0000000000000000 ) ) ;
#7691 = DIRECTION ( 'NONE',  ( 1.460819769243627131E-16, 0.000000000000000000, -1.000000000000000000 ) ) ;
#7692 = ORIENTED_EDGE ( 'NONE', *, *, #10333, .T. ) ;
#7693 = UNCERTAINTY_MEASURE_WITH_UNIT (LENGTH_MEASURE( 1.000000000000000082E-05 ), #8397, 'distance_accuracy_value', 'NONE');
#7694 = LINE ( 'NONE', #2148, #7618 ) ;
#7695 = ORIENTED_EDGE ( 'NONE', *, *, #2696, .T. ) ;
#7696 = DIRECTION ( 'NONE',  ( 1.000000000000000000, 2.312964634635740689E-15, 0.000000000000000000 ) ) ;
#7697 = CARTESIAN_POINT ( 'NONE',  ( 3.500000000000000000, 0.000000000000000000, 0.000000000000000000 ) ) ;
#7698 = DIRECTION ( 'NONE',  ( 0.8571673013836776933, 1.049727191973295533E-16, -0.5150380737757388472 ) ) ;
#7699 = EDGE_CURVE ( 'NONE', #2880, #4156, #9560, .T. ) ;
#7700 = ORIENTED_EDGE ( 'NONE', *, *, #7139, .T. ) ;
#7701 = LINE ( 'NONE', #4105, #10612 ) ;
#7702 = EDGE_LOOP ( 'NONE', ( #3286, #11197, #4720, #6668 ) ) ;
#7703 = VERTEX_POINT ( 'NONE', #11615 ) ;
#7704 = LINE ( 'NONE', #3139, #13952 ) ;
#7705 = CARTESIAN_POINT ( 'NONE',  ( 0.5590169943749477843, 0.000000000000000000, 0.000000000000000000 ) ) ;
#7706 = CARTESIAN_POINT ( 'NONE',  ( -2.687328764639638656, 3.067272167851286202, -0.05923475698270370959 ) ) ;
#7707 = ORIENTED_EDGE ( 'NONE', *, *, #10009, .F. ) ;
#7708 = ORIENTED_EDGE ( 'NONE', *, *, #3683, .T. ) ;
#7709 = DIRECTION ( 'NONE',  ( 0.000000000000000000, -1.000000000000000000, 0.000000000000000000 ) ) ;
#7710 = LINE ( 'NONE', #5505, #5194 ) ;
#7711 = DIRECTION ( 'NONE',  ( -0.2873478855663453291, -0.9578262852211513190, -3.835990623682899812E-15 ) ) ;
#7712 = FACE_OUTER_BOUND ( 'NONE', #4326, .T. ) ;
#7713 = FACE_OUTER_BOUND ( 'NONE', #8044, .T. ) ;
#7714 = SURFACE_STYLE_FILL_AREA ( #6472 ) ;
#7715 = EDGE_CURVE ( 'NONE', #4117, #3851, #7284, .T. ) ;
#7716 = ORIENTED_EDGE ( 'NONE', *, *, #9732, .T. ) ;
#7717 = CARTESIAN_POINT ( 'NONE',  ( 609.8294541519869654, 189.4056243435263980, 189.7329333695814739 ) ) ;
#7718 = EDGE_LOOP ( 'NONE', ( #7047, #509, #8408, #8126 ) ) ;
#7719 = DIRECTION ( 'NONE',  ( -1.000000000000000000, -0.000000000000000000, 0.000000000000000000 ) ) ;
#7720 = CIRCLE ( 'NONE', #7249, 4.000000000000000000 ) ;
#7721 = VERTEX_POINT ( 'NONE', #10446 ) ;
#7722 = VECTOR ( 'NONE', #13754, 1000.000000000000000 ) ;
#7723 = EDGE_CURVE ( 'NONE', #4487, #2113, #6600, .T. ) ;
#7724 = AXIS2_PLACEMENT_3D ( 'NONE', #6945, #11442, #10338 ) ;
#7725 = DIRECTION ( 'NONE',  ( 1.000000000000000000, 0.000000000000000000, 0.000000000000000000 ) ) ;
#7726 = CARTESIAN_POINT ( 'NONE',  ( 610.0000000000000000, 0.000000000000000000, 210.0000000000000000 ) ) ;
#7727 = ORIENTED_EDGE ( 'NONE', *, *, #3637, .F. ) ;
#7728 = FACE_OUTER_BOUND ( 'NONE', #675, .T. ) ;
#7729 = DIRECTION ( 'NONE',  ( 0.000000000000000000, 0.000000000000000000, 1.000000000000000000 ) ) ;
#7730=STYLED_ITEM('',(#14688),#2587);
#7731 = AXIS2_PLACEMENT_3D ( 'NONE', #4115, #12197, #10960 ) ;
#7732 = CARTESIAN_POINT ( 'NONE',  ( 707.0389973793288618, 162.8315651648156290, 150.0000000000013358 ) ) ;
#7733 = ADVANCED_FACE ( 'NONE', ( #2692 ), #2917, .F. ) ;
#7734 = ORIENTED_EDGE ( 'NONE', *, *, #6173, .T. ) ;
#7735 = ORIENTED_EDGE ( 'NONE', *, *, #3066, .F. ) ;
#7736 = ADVANCED_BREP_SHAPE_REPRESENTATION ( '', ( #2529, #9440 ), #13 ) ;
#7737 = ORIENTED_EDGE ( 'NONE', *, *, #5349, .F. ) ;
#7738 = CARTESIAN_POINT ( 'NONE',  ( 0.3572655899081578768, -4.618802153516999631, -3.329030144205522754E-16 ) ) ;
#7739 = CIRCLE ( 'NONE', #13392, 2.649999999999985700 ) ;
#7740 = ADVANCED_FACE ( 'NONE', ( #8813 ), #977, .T. ) ;
#7742 = VECTOR ( 'NONE', #14486, 1000.000000000000000 ) ;
#7741 = DIRECTION ( 'NONE',  ( -1.000000000000000000, 0.000000000000000000, 0.000000000000000000 ) ) ;
#7743 = CARTESIAN_POINT ( 'NONE',  ( 2.500000000000000000, -2.629050547790028551E-15, -2.041999999999999815 ) ) ;
#7744 = ADVANCED_FACE ( 'NONE', ( #824 ), #14276, .F. ) ;
#7745 = PRODUCT_RELATED_PRODUCT_CATEGORY ( 'part', '', ( #7374 ) ) ;
#7746 = DIRECTION ( 'NONE',  ( -0.000000000000000000, -0.000000000000000000, -1.000000000000000000 ) ) ;
#7747 = CARTESIAN_POINT ( 'NONE',  ( 0.8808064505786590281, 6.997019658119588925, -5.875704392892181716 ) ) ;
#7748 = FACE_OUTER_BOUND ( 'NONE', #4657, .T. ) ;
#7749 = FACE_OUTER_BOUND ( 'NONE', #6523, .T. ) ;
#7750 = ORIENTED_EDGE ( 'NONE', *, *, #1954, .F. ) ;
#7751 = COLOUR_RGB ( '',0.8941176470588234615, 0.8941176470588234615, 0.8941176470588234615 ) ;
#7752 = VECTOR ( 'NONE', #7771, 1000.000000000000000 ) ;
#7753 = CARTESIAN_POINT ( 'NONE',  ( 0.000000000000000000, 0.000000000000000000, 0.000000000000000000 ) ) ;
#7754 = FACE_OUTER_BOUND ( 'NONE', #13833, .T. ) ;
#7755 = PRODUCT_CONTEXT ( 'NONE', #7830, 'mechanical' ) ;
#7756 = DIRECTION ( 'NONE',  ( -0.000000000000000000, -0.000000000000000000, -1.000000000000000000 ) ) ;
#7757 = ORIENTED_EDGE ( 'NONE', *, *, #14531, .T. ) ;
#7758 = ORIENTED_EDGE ( 'NONE', *, *, #2161, .F. ) ;
#7759 = DIRECTION ( 'NONE',  ( 0.000000000000000000, 0.000000000000000000, -1.000000000000000000 ) ) ;
#7760 = DIRECTION ( 'NONE',  ( -9.223531621143024916E-30, 2.767059486342909086E-30, 1.000000000000000000 ) ) ;
#7761=STYLED_ITEM('',(#14674),#7105);
#7762 = DIRECTION ( 'NONE',  ( -1.000000000000000000, 0.000000000000000000, 0.000000000000000000 ) ) ;
#7763 = VECTOR ( 'NONE', #362, 1000.000000000000114 ) ;
#7764 = CARTESIAN_POINT ( 'NONE',  ( 6.500000000000000000, -2.501851166488383349, -5.848636054922036642 ) ) ;
#7765 = VERTEX_POINT ( 'NONE', #14343 ) ;
#7766 = DIRECTION ( 'NONE',  ( 1.000000000000000000, 0.000000000000000000, 0.000000000000000000 ) ) ;
#7767 = ORIENTED_EDGE ( 'NONE', *, *, #704, .F. ) ;
#7768 = MECHANICAL_DESIGN_GEOMETRIC_PRESENTATION_REPRESENTATION (  '', ( #11527 ), #12714 ) ;
#7769 = EDGE_CURVE ( 'NONE', #4552, #10951, #678, .T. ) ;
#7770 = CARTESIAN_POINT ( 'NONE',  ( 148.9991633467111569, 386.6211705227183870, 187.0000000000000568 ) ) ;
#7771 = DIRECTION ( 'NONE',  ( 1.000000000000000000, 0.000000000000000000, 0.000000000000000000 ) ) ;
#7772 = SURFACE_STYLE_USAGE ( .BOTH. , #4531 ) ;
#7773 = AXIS2_PLACEMENT_3D ( 'NONE', #5267, #2820, #11821 ) ;
#7774 = EDGE_CURVE ( 'NONE', #9996, #2446, #11669, .T. ) ;
#7775 = CARTESIAN_POINT ( 'NONE',  ( 6.244297270354683960, 1.800816419761795034E-11, 5.105276777067893512 ) ) ;
#7776 = CIRCLE ( 'NONE', #3294, 6.975000000000000533 ) ;
#7777 = ORIENTED_EDGE ( 'NONE', *, *, #4228, .F. ) ;
#7778 = ORIENTED_EDGE ( 'NONE', *, *, #4147, .T. ) ;
#7779 = CARTESIAN_POINT ( 'NONE',  ( 0.05140428708382503709, 3.841181488860375470, -3.346878500200758833 ) ) ;
#7780 = DIRECTION ( 'NONE',  ( 0.000000000000000000, -1.224646799147353700E-16, 1.000000000000000000 ) ) ;
#7781 = VECTOR ( 'NONE', #14059, 1000.000000000000000 ) ;
#7782 = CARTESIAN_POINT ( 'NONE',  ( 4.000000000000000000, -2.471525695159793035, -3.686886880705770864 ) ) ;
#7783 = EDGE_LOOP ( 'NONE', ( #2210, #9366 ) ) ;
#7784 = AXIS2_PLACEMENT_3D ( 'NONE', #1644, #9329, #2461 ) ;
#7785 = ADVANCED_FACE ( 'NONE', ( #4165 ), #8954, .T. ) ;
#7786 = ORIENTED_EDGE ( 'NONE', *, *, #3437, .F. ) ;
#7787 = DIRECTION ( 'NONE',  ( -1.000000000000000000, -0.000000000000000000, -0.000000000000000000 ) ) ;
#7788 = CARTESIAN_POINT ( 'NONE',  ( 6.534838248920900483, -5.903531555104837736, 5.201568163584232486E-16 ) ) ;
#7789 = DIRECTION ( 'NONE',  ( -1.000000000000000000, -0.000000000000000000, -0.000000000000000000 ) ) ;
#7790 = DIRECTION ( 'NONE',  ( -1.000000000000000000, 0.000000000000000000, 0.000000000000000000 ) ) ;
#7791 = CARTESIAN_POINT ( 'NONE',  ( -8.074769166705396017, 378.0965165842501392, -187.0000000000000284 ) ) ;
#7792 = VECTOR ( 'NONE', #3124, 1000.000000000000000 ) ;
#7793 = ORIENTED_EDGE ( 'NONE', *, *, #7862, .F. ) ;
#7794 = VECTOR ( 'NONE', #9684, 1000.000000000000227 ) ;
#7795 = DIRECTION ( 'NONE',  ( 0.000000000000000000, 0.000000000000000000, 1.000000000000000000 ) ) ;
#7796 = ORIENTED_EDGE ( 'NONE', *, *, #970, .F. ) ;
#7797 = ORIENTED_EDGE ( 'NONE', *, *, #10983, .F. ) ;
#7798 = CARTESIAN_POINT ( 'NONE',  ( 0.000000000000000000, 0.000000000000000000, 0.000000000000000000 ) ) ;
#7799 = AXIS2_PLACEMENT_3D ( 'NONE', #8895, #12290, #2183 ) ;
#7800 = VECTOR ( 'NONE', #2347, 999.9999999999998863 ) ;
#7801 = EDGE_LOOP ( 'NONE', ( #11270, #10752 ) ) ;
#7802 = CARTESIAN_POINT ( 'NONE',  ( -1.399999999999998579, 0.000000000000000000, 0.000000000000000000 ) ) ;
#7803 = VECTOR ( 'NONE', #13662, 1000.000000000000227 ) ;
#7804 = EDGE_CURVE ( 'NONE', #10481, #14303, #9189, .T. ) ;
#7805 = DIRECTION ( 'NONE',  ( -0.2873478855663453846, -0.9578262852211513190, -0.000000000000000000 ) ) ;
#7806 = EDGE_LOOP ( 'NONE', ( #2558, #5418, #9577, #7637 ) ) ;
#7807 = CARTESIAN_POINT ( 'NONE',  ( 0.3117969352650126202, 2.419842229202155082, 4.999999999999999112 ) ) ;
#7808 = FACE_OUTER_BOUND ( 'NONE', #5779, .T. ) ;
#7809 = VECTOR ( 'NONE', #2485, 1000.000000000000114 ) ;
#7810 = COLOUR_RGB ( '',0.8941176470588234615, 0.8941176470588234615, 0.8941176470588234615 ) ;
#7811 = DIRECTION ( 'NONE',  ( 1.000000000000000000, 9.498873539028489960E-17, 0.000000000000000000 ) ) ;
#7812 = FACE_OUTER_BOUND ( 'NONE', #3773, .T. ) ;
#7813 = ORIENTED_EDGE ( 'NONE', *, *, #10954, .F. ) ;
#7814 = CARTESIAN_POINT ( 'NONE',  ( -1.968420164455561244E-13, 3.855132749030457888E-14, 179.7999999999994714 ) ) ;
#7815 = ORIENTED_EDGE ( 'NONE', *, *, #11747, .T. ) ;
#7816 = AXIS2_PLACEMENT_3D ( 'NONE', #14238, #10014, #11043 ) ;
#7817 = AXIS2_PLACEMENT_3D ( 'NONE', #310, #13918, #7341 ) ;
#7818 = EDGE_LOOP ( 'NONE', ( #11540, #754, #13242, #3696 ) ) ;
#7819 = DIRECTION ( 'NONE',  ( -0.000000000000000000, -0.000000000000000000, -1.000000000000000000 ) ) ;
#7820 = DIRECTION ( 'NONE',  ( -0.000000000000000000, -0.000000000000000000, -1.000000000000000000 ) ) ;
#7821 = EDGE_CURVE ( 'NONE', #5128, #7703, #7701, .T. ) ;
#7822 = LINE ( 'NONE', #12160, #1187 ) ;
#7823 = CIRCLE ( 'NONE', #10182, 7.500000000000062172 ) ;
#7824 = LINE ( 'NONE', #9815, #7570 ) ;
#7825 = EDGE_CURVE ( 'NONE', #12031, #10699, #5660, .T. ) ;
#7826 = DIRECTION ( 'NONE',  ( -1.000802005371232860E-15, 0.000000000000000000, -1.000000000000000000 ) ) ;
#7827 = FACE_OUTER_BOUND ( 'NONE', #13644, .T. ) ;
#7828 = CARTESIAN_POINT ( 'NONE',  ( -3.755786496842903988E-16, -7.505553499465146494, -8.000000000000000000 ) ) ;
#7829 = ADVANCED_FACE ( 'NONE', ( #7559 ), #4966, .T. ) ;
#7830 = APPLICATION_CONTEXT ( 'automotive_design' ) ;
#7831 = EDGE_LOOP ( 'NONE', ( #9062, #5483 ) ) ;
#7832 = ADVANCED_FACE ( 'NONE', ( #4022 ), #2982, .T. ) ;
#7833 = CARTESIAN_POINT ( 'NONE',  ( -5.589124336235484769, -4.278671059406953248, -6.219623095964403880 ) ) ;
#7834 = FACE_OUTER_BOUND ( 'NONE', #2254, .T. ) ;
#7835 = CONTEXT_DEPENDENT_SHAPE_REPRESENTATION ( #8580, #2753 ) ;
#7837 = EDGE_CURVE ( 'NONE', #12356, #2837, #9758, .T. ) ;
#7836 = CARTESIAN_POINT ( 'NONE',  ( 6.837824896291514243, 3.947820044545427454, -6.564402953523716278 ) ) ;
#7838 = ORIENTED_EDGE ( 'NONE', *, *, #3943, .T. ) ;
#7839 = EDGE_LOOP ( 'NONE', ( #3229, #10978, #12988, #14318 ) ) ;
#7840 = VECTOR ( 'NONE', #8246, 1000.000000000000000 ) ;
#7841 = DIRECTION ( 'NONE',  ( 1.000000000000000000, 0.000000000000000000, 0.000000000000000000 ) ) ;
#7842 = CARTESIAN_POINT ( 'NONE',  ( 148.9991633467111569, 386.6211705227183870, -190.0000000000000000 ) ) ;
#7843 = CARTESIAN_POINT ( 'NONE',  ( 650.0000000000000000, 175.0000000000000568, 210.0000000000000000 ) ) ;
#7844 = PRODUCT_DEFINITION_FORMATION_WITH_SPECIFIED_SOURCE ( 'ANY', '', #14090, .NOT_KNOWN. ) ;
#7845 = DIRECTION ( 'NONE',  ( 1.000000000000000000, 0.000000000000000000, -0.000000000000000000 ) ) ;
#7846 = EDGE_LOOP ( 'NONE', ( #1495, #7316, #10878 ) ) ;
#7847 = UNCERTAINTY_MEASURE_WITH_UNIT (LENGTH_MEASURE( 1.000000000000000082E-05 ), #7290, 'distance_accuracy_value', 'NONE');
#7848 = LINE ( 'NONE', #12333, #2900 ) ;
#7849 = ORIENTED_EDGE ( 'NONE', *, *, #10962, .T. ) ;
#7850 = ADVANCED_FACE ( 'NONE', ( #11090 ), #5342, .F. ) ;
#7851 = EDGE_CURVE ( 'NONE', #5305, #8880, #9841, .T. ) ;
#7852 = CARTESIAN_POINT ( 'NONE',  ( 5.000000000000002665, 0.000000000000000000, -2.700000000000000622 ) ) ;
#7853 = DIRECTION ( 'NONE',  ( -1.000000000000000000, 0.000000000000000000, 0.000000000000000000 ) ) ;
#7854 = B_SPLINE_CURVE_WITH_KNOTS ( 'NONE', 3,
 ( #11198, #4413, #12300, #13200, #3016, #12010, #1907, #6420 ),
 .UNSPECIFIED., .F., .F.,
 ( 4, 2, 2, 4 ),
 ( 0.000000000000000000, 0.001493104274552339720, 0.002986208549104679439, 0.005972417098209361480 ),
 .UNSPECIFIED. ) ;
#7855 = CARTESIAN_POINT ( 'NONE',  ( -9.137956343300736251, 416.3137853645750397, -184.7999999999999829 ) ) ;
#7856 = ORIENTED_EDGE ( 'NONE', *, *, #1784, .F. ) ;
#7857 = EDGE_LOOP ( 'NONE', ( #11855, #3361, #11167, #8227 ) ) ;
#7858 = CARTESIAN_POINT ( 'NONE',  ( 610.8620436566991430, 188.5525593289318920, -187.0000000000000000 ) ) ;
#7859 = DIRECTION ( 'NONE',  ( -0.000000000000000000, 1.000000000000000000, 1.224646799147353207E-16 ) ) ;
#7860 = CONICAL_SURFACE ( 'NONE', #9031, 5.560781378645573980, 1.221730476396046816 ) ;
#7861 = CLOSED_SHELL ( 'NONE', ( #4831, #11356, #14544, #3220, #9967, #8090, #3300, #4685, #10916, #5044, #8919, #8566, #8713, #1723, #2083, #699, #13078, #12124, #11696, #13971, #12097, #1959, #11885, #744, #7185, #2683, #2212, #12288, #12831 ) ) ;
#7862 = EDGE_CURVE ( 'NONE', #10329, #3163, #4484, .T. ) ;
#7863 = CARTESIAN_POINT ( 'NONE',  ( 2.999999999999999112, 4.000000000000000000, 0.000000000000000000 ) ) ;
#7864 = EDGE_LOOP ( 'NONE', ( #10203, #14277 ) ) ;
#7865 = LINE ( 'NONE', #7631, #11851 ) ;
#7866 = CARTESIAN_POINT ( 'NONE',  ( 609.8668404561643683, 185.6877074168924935, -185.4847245573741930 ) ) ;
#7867 = DIRECTION ( 'NONE',  ( 0.000000000000000000, 0.000000000000000000, -1.000000000000000000 ) ) ;
#7868 = CARTESIAN_POINT ( 'NONE',  ( 655.0000000000000000, 160.0000000000000284, -187.5000000000000000 ) ) ;
#7869 = DIRECTION ( 'NONE',  ( 0.000000000000000000, -0.000000000000000000, -1.000000000000000000 ) ) ;
#7870 = SURFACE_STYLE_FILL_AREA ( #13388 ) ;
#7871 = EDGE_LOOP ( 'NONE', ( #12347, #14170, #2149, #2274 ) ) ;
#7872 = FACE_OUTER_BOUND ( 'NONE', #12060, .T. ) ;
#7873 = ORIENTED_EDGE ( 'NONE', *, *, #11605, .F. ) ;
#7874 = ORIENTED_EDGE ( 'NONE', *, *, #6899, .T. ) ;
#7875 = CARTESIAN_POINT ( 'NONE',  ( 6.507056081706568129, -2.993351035583803110, -4.999999999999999112 ) ) ;
#7876 = ORIENTED_EDGE ( 'NONE', *, *, #5314, .F. ) ;
#7877 = DIRECTION ( 'NONE',  ( 0.000000000000000000, 0.000000000000000000, -1.000000000000000000 ) ) ;
#7878 = CARTESIAN_POINT ( 'NONE',  ( 0.000000000000000000, 0.000000000000000000, 0.000000000000000000 ) ) ;
#7879 = ORIENTED_EDGE ( 'NONE', *, *, #10760, .T. ) ;
#7880 = DIRECTION ( 'NONE',  ( -0.000000000000000000, -0.000000000000000000, 1.000000000000000000 ) ) ;
#7881 = LINE ( 'NONE', #12366, #13188 ) ;
#7882 = FACE_OUTER_BOUND ( 'NONE', #1281, .T. ) ;
#7883 = LINE ( 'NONE', #11413, #8312 ) ;
#7884 = ORIENTED_EDGE ( 'NONE', *, *, #4958, .F. ) ;
#7885 = CARTESIAN_POINT ( 'NONE',  ( 650.0000000000000000, 175.0000000000000568, 190.0000000000000000 ) ) ;
#7886 = VERTEX_POINT ( 'NONE', #7917 ) ;
#7887 = EDGE_CURVE ( 'NONE', #293, #13306, #6952, .T. ) ;
#7888 = EDGE_LOOP ( 'NONE', ( #5005, #5049, #8517, #9077 ) ) ;
#7889 = CARTESIAN_POINT ( 'NONE',  ( 9.498873539028489220E-16, -10.00000000000000000, 190.0000000000000000 ) ) ;
#7890 = CARTESIAN_POINT ( 'NONE',  ( 139.8040310085880833, 355.9707293956415697, -210.0000000000000000 ) ) ;
#7891 = DIRECTION ( 'NONE',  ( 0.000000000000000000, 0.000000000000000000, -1.000000000000000000 ) ) ;
#7892 = DIRECTION ( 'NONE',  ( 0.000000000000000000, 0.000000000000000000, -1.000000000000000000 ) ) ;
#7893 = CARTESIAN_POINT ( 'NONE',  ( -8.074769166705396017, 378.0965165842501392, 187.0000000000000284 ) ) ;
#7894 = DIRECTION ( 'NONE',  ( 0.000000000000000000, -0.000000000000000000, 1.000000000000000000 ) ) ;
#7895 = VECTOR ( 'NONE', #9753, 1000.000000000000000 ) ;
#7896 = DIRECTION ( 'NONE',  ( 0.000000000000000000, 0.000000000000000000, -1.000000000000000000 ) ) ;
#7897 = VERTEX_POINT ( 'NONE', #5491 ) ;
#7898 = DIRECTION ( 'NONE',  ( 0.2873478855663477161, 0.9578262852211506528, 0.000000000000000000 ) ) ;
#7899 = CARTESIAN_POINT ( 'NONE',  ( 6.534224484704354907, -5.901860969583196059, 7.986458555526148407E-15 ) ) ;
#7900 = APPLICATION_PROTOCOL_DEFINITION ( 'draft international standard', 'automotive_design', 1998, #13660 ) ;
#7901 = EDGE_CURVE ( 'NONE', #4197, #12301, #2155, .T. ) ;
#7902 = CARTESIAN_POINT ( 'NONE',  ( 6.539198257602124364, 3.775407874310915179, -6.286450516131049326 ) ) ;
#7903 = EDGE_LOOP ( 'NONE', ( #1751, #3084, #8716, #1746 ) ) ;
#7904 = ORIENTED_EDGE ( 'NONE', *, *, #11771, .T. ) ;
#7905 = CYLINDRICAL_SURFACE ( 'NONE', #4680, 2.700000000000000178 ) ;
#7906 = DIRECTION ( 'NONE',  ( -0.2873478855663477161, -0.9578262852211506528, 0.000000000000000000 ) ) ;
#7907 = ADVANCED_FACE ( 'NONE', ( #13531, #9987 ), #2289, .F. ) ;
#7908 = DIRECTION ( 'NONE',  ( 0.000000000000000000, 1.000000000000000000, 0.000000000000000000 ) ) ;
#7909 = ADVANCED_FACE ( 'NONE', ( #3569 ), #1192, .F. ) ;
#7910 = DIRECTION ( 'NONE',  ( -0.9578262852211513190, 0.2873478855663453846, 0.000000000000000000 ) ) ;
#7911 = EDGE_CURVE ( 'NONE', #1238, #4931, #5772, .T. ) ;
#7912 = FACE_OUTER_BOUND ( 'NONE', #2317, .T. ) ;
#7913 = VERTEX_POINT ( 'NONE', #8872 ) ;
#7914 = CARTESIAN_POINT ( 'NONE',  ( -4.000000000000000888, -1.539600717839011201, -3.300726591567081591 ) ) ;
#7915 = DIRECTION ( 'NONE',  ( -0.000000000000000000, -1.000000000000000000, -0.000000000000000000 ) ) ;
#7916 =( NAMED_UNIT ( * ) SI_UNIT ( $, .STERADIAN. ) SOLID_ANGLE_UNIT ( ) );
#7917 = CARTESIAN_POINT ( 'NONE',  ( 640.2500000000000000, 160.0000000000000284, 190.0000000000000284 ) ) ;
#7918 = ORIENTED_EDGE ( 'NONE', *, *, #7246, .T. ) ;
#7919 = ORIENTED_EDGE ( 'NONE', *, *, #7397, .F. ) ;
#7920 = CARTESIAN_POINT ( 'NONE',  ( 1.411581201560190495E-15, 4.862606272033091592, -3.745885042887436622 ) ) ;
#7921 = CARTESIAN_POINT ( 'NONE',  ( 604.3113219698374223, -181.2933965909553535, -177.5999999999989143 ) ) ;
#7922 = EDGE_CURVE ( 'NONE', #2271, #11363, #5704, .T. ) ;
#7923 = DIRECTION ( 'NONE',  ( 1.000000000000000000, 0.000000000000000000, 0.000000000000000000 ) ) ;
#7924 = ORIENTED_EDGE ( 'NONE', *, *, #6620, .F. ) ;
#7925 = EDGE_CURVE ( 'NONE', #2358, #7390, #14557, .T. ) ;
#7926 = ORIENTED_EDGE ( 'NONE', *, *, #14145, .T. ) ;
#7927 = CARTESIAN_POINT ( 'NONE',  ( 148.9991633467111569, 386.6211705227183870, 190.0000000000000000 ) ) ;
#7928 = DIRECTION ( 'NONE',  ( -0.000000000000000000, -0.000000000000000000, 1.000000000000000000 ) ) ;
#7929 = FACE_OUTER_BOUND ( 'NONE', #4415, .T. ) ;
#7930 = DIRECTION ( 'NONE',  ( 0.000000000000000000, 0.000000000000000000, -1.000000000000000000 ) ) ;
#7931 = ORIENTED_EDGE ( 'NONE', *, *, #11301, .T. ) ;
#7932 = DIRECTION ( 'NONE',  ( -0.000000000000000000, -0.000000000000000000, 1.000000000000000000 ) ) ;
#7933 = ORIENTED_EDGE ( 'NONE', *, *, #2164, .F. ) ;
#7934 = EDGE_LOOP ( 'NONE', ( #857, #385 ) ) ;
#7935 = PLANE ( 'NONE',  #723 ) ;
#7936 = ORIENTED_EDGE ( 'NONE', *, *, #12847, .F. ) ;
#7937 = CARTESIAN_POINT ( 'NONE',  ( 641.0000000000000000, 166.0000000000000284, -187.5000000000000000 ) ) ;
#7938 = DIRECTION ( 'NONE',  ( -1.000000000000000000, -0.000000000000000000, -0.000000000000000000 ) ) ;
#7939 = VERTEX_POINT ( 'NONE', #1274 ) ;
#7940 = CARTESIAN_POINT ( 'NONE',  ( 6.371919382990604674, 1.972754410575519035, 5.108792907957607099 ) ) ;
#7941 = CARTESIAN_POINT ( 'NONE',  ( 137.1540310085880776, 355.9707293956415697, 190.0000000000000000 ) ) ;
#7942 = DIRECTION ( 'NONE',  ( -7.885106708985460438E-16, 0.000000000000000000, -1.000000000000000000 ) ) ;
#7943 = DIRECTION ( 'NONE',  ( 1.000000000000000000, 0.000000000000000000, 0.000000000000000000 ) ) ;
#7944 = VERTEX_POINT ( 'NONE', #9094 ) ;
#7945 = FACE_OUTER_BOUND ( 'NONE', #4481, .T. ) ;
#7946 = AXIS2_PLACEMENT_3D ( 'NONE', #7176, #5925, #1419 ) ;
#7947 = ORIENTED_EDGE ( 'NONE', *, *, #11515, .T. ) ;
#7948 = ORIENTED_EDGE ( 'NONE', *, *, #12602, .F. ) ;
#7949 = CARTESIAN_POINT ( 'NONE',  ( 4.444974277458119793, -4.939246403833736032, -5.720331885005374595 ) ) ;
#7950 = CARTESIAN_POINT ( 'NONE',  ( 629.0000000000000000, 154.0000000000000284, 187.5000000000000000 ) ) ;
#7951 = DIRECTION ( 'NONE',  ( 1.000000000000000000, 0.000000000000000000, 0.000000000000000000 ) ) ;
#7952 = CIRCLE ( 'NONE', #11256, 2.649999999999985700 ) ;
#7953 = PRODUCT_DEFINITION_SHAPE ( 'NONE', 'NONE',  #14638 ) ;
#7954 = EDGE_CURVE ( 'NONE', #2701, #3667, #9046, .T. ) ;
#7955 = DIRECTION ( 'NONE',  ( 1.000000000000000000, 0.000000000000000000, 0.000000000000000000 ) ) ;
#7956 = EDGE_CURVE ( 'NONE', #6358, #13114, #10379, .T. ) ;
#7957 = DIRECTION ( 'NONE',  ( -1.063400795443706786E-15, 3.190202386331118779E-16, 1.000000000000000000 ) ) ;
#7958 = PLANE ( 'NONE',  #8260 ) ;
#7959 = CARTESIAN_POINT ( 'NONE',  ( 1.400000000000001910, 6.184466335694134054E-16, 5.000000000000000000 ) ) ;
#7960 = ORIENTED_EDGE ( 'NONE', *, *, #12950, .F. ) ;
#7961 = CARTESIAN_POINT ( 'NONE',  ( 6.196878017913834746, -5.292377467571577121, -0.8333333333333333703 ) ) ;
#7962 = FACE_OUTER_BOUND ( 'NONE', #11350, .T. ) ;
#7963 = FACE_OUTER_BOUND ( 'NONE', #5644, .T. ) ;
#7964 = ORIENTED_EDGE ( 'NONE', *, *, #12675, .T. ) ;
#7965 = AXIS2_PLACEMENT_3D ( 'NONE', #7346, #10674, #6091 ) ;
#7966 = CARTESIAN_POINT ( 'NONE',  ( -1.250000000000000000, -6.429618962271402616, -1.000000000000000000 ) ) ;
#7967 = AXIS2_PLACEMENT_3D ( 'NONE', #2913, #4101, #1648 ) ;
#7968 = EDGE_LOOP ( 'NONE', ( #13015, #13096, #3292, #12204 ) ) ;
#7969 = ORIENTED_EDGE ( 'NONE', *, *, #157, .T. ) ;
#7970 = LINE ( 'NONE', #2211, #6610 ) ;
#7971 = CARTESIAN_POINT ( 'NONE',  ( 3.700000000000000178, 3.061616997868383634E-16, -2.500000000000000444 ) ) ;
#7972 = EDGE_CURVE ( 'NONE', #7687, #2732, #6732, .T. ) ;
#7973 = CARTESIAN_POINT ( 'NONE',  ( 139.8040310085880833, 355.9707293956415697, 187.0000000000000000 ) ) ;
#7974 = AXIS2_PLACEMENT_3D ( 'NONE', #6457, #2978, #9914 ) ;
#7975 = CARTESIAN_POINT ( 'NONE',  ( 6.092449800118536984, -4.833012432206698072, -1.628976913805976423 ) ) ;
#7976 = ORIENTED_EDGE ( 'NONE', *, *, #2986, .F. ) ;
#7977 = DIRECTION ( 'NONE',  ( -1.000000000000000000, -0.000000000000000000, -0.000000000000000000 ) ) ;
#7978 = CARTESIAN_POINT ( 'NONE',  ( 133.6739427831727198, 370.3381236739588758, -210.0000000000000000 ) ) ;
#7979 = EDGE_CURVE ( 'NONE', #3065, #11111, #3597, .T. ) ;
#7980 = DIRECTION ( 'NONE',  ( 1.000000000000000000, 0.000000000000000000, 0.000000000000000000 ) ) ;
#7981 = ORIENTED_EDGE ( 'NONE', *, *, #8532, .T. ) ;
#7982 = VERTEX_POINT ( 'NONE', #8947 ) ;
#7983 = CARTESIAN_POINT ( 'NONE',  ( 4.204015924366189871, -1.626724848190933548, -3.610627190413393084 ) ) ;
#7984 = AXIS2_PLACEMENT_3D ( 'NONE', #9508, #12544, #4736 ) ;
#7985 = DIRECTION ( 'NONE',  ( 0.03086419753086420623, 0.9995235871707959241, -0.000000000000000000 ) ) ;
#7986 = CARTESIAN_POINT ( 'NONE',  ( -4.204015924366189871, 1.626724848190922446, -3.610627190413390419 ) ) ;
#7987 = ADVANCED_FACE ( 'NONE', ( #13456 ), #3352, .T. ) ;
#7988 = VECTOR ( 'NONE', #6491, 1000.000000000000114 ) ;
#7989 = VERTEX_POINT ( 'NONE', #7855 ) ;
#7990 = ORIENTED_EDGE ( 'NONE', *, *, #13466, .F. ) ;
#7991 = CARTESIAN_POINT ( 'NONE',  ( 610.3661002516460030, 189.1614810556852717, -186.1520027839448232 ) ) ;
#7992 = LINE ( 'NONE', #13541, #11547 ) ;
#7993 = CIRCLE ( 'NONE', #6347, 3.399999999999999911 ) ;
#7994 = VECTOR ( 'NONE', #13334, 1000.000000000000000 ) ;
#7995 = LINE ( 'NONE', #8073, #10085 ) ;
#7996 = CARTESIAN_POINT ( 'NONE',  ( 228.5935732249378987, 306.3651924111343305, 177.6000000000001648 ) ) ;
#7997 =( LENGTH_UNIT ( ) NAMED_UNIT ( * ) SI_UNIT ( .MILLI., .METRE. ) );
#7998 = EDGE_CURVE ( 'NONE', #6317, #5365, #11325, .T. ) ;
#7999 = VERTEX_POINT ( 'NONE', #12402 ) ;
#8000 = EDGE_CURVE ( 'NONE', #9573, #809, #2367, .T. ) ;
#8001 = CYLINDRICAL_SURFACE ( 'NONE', #12014, 5.199999999999715961 ) ;
#8002 = VERTEX_POINT ( 'NONE', #13593 ) ;
#8003 = ORIENTED_EDGE ( 'NONE', *, *, #7432, .F. ) ;
#8004 = CARTESIAN_POINT ( 'NONE',  ( 6.499999999999999112, -3.752776749732576356, -0.8000000000000003775 ) ) ;
#8005 = AXIS2_PLACEMENT_3D ( 'NONE', #13785, #6763, #5666 ) ;
#8006 = EDGE_CURVE ( 'NONE', #9048, #681, #2665, .T. ) ;
#8007 = VERTEX_POINT ( 'NONE', #10490 ) ;
#8008 = AXIS2_PLACEMENT_3D ( 'NONE', #5883, #11353, #8241 ) ;
#8009 = AXIS2_PLACEMENT_3D ( 'NONE', #12817, #5872, #10378 ) ;
#8010 = FACE_OUTER_BOUND ( 'NONE', #359, .T. ) ;
#8011 = CARTESIAN_POINT ( 'NONE',  ( 3.999999999999999112, 4.898587196589411843E-16, -7.974599999999998801 ) ) ;
#8012 = AXIS2_PLACEMENT_3D ( 'NONE', #7842, #11373, #6941 ) ;
#8013 = VERTEX_POINT ( 'NONE', #11597 ) ;
#8014 = CARTESIAN_POINT ( 'NONE',  ( 650.0000000000000000, 145.0000000000000568, 190.0000000000000000 ) ) ;
#8015 = CARTESIAN_POINT ( 'NONE',  ( 611.4942090049451053, 232.4210031920598567, -190.0000000000000000 ) ) ;
#8016 = CARTESIAN_POINT ( 'NONE',  ( 2.500000000000000444, 0.000000000000000000, -25.03750572909317285 ) ) ;
#8017 = PLANE ( 'NONE',  #7616 ) ;
#8018 =( LENGTH_UNIT ( ) NAMED_UNIT ( * ) SI_UNIT ( .MILLI., .METRE. ) );
#8019 = VERTEX_POINT ( 'NONE', #7312 ) ;
#8020 = ADVANCED_FACE ( 'NONE', ( #1555 ), #11662, .F. ) ;
#8021 = AXIS2_PLACEMENT_3D ( 'NONE', #10157, #12430, #10229 ) ;
#8022 = AXIS2_PLACEMENT_3D ( 'NONE', #5157, #5089, #8392 ) ;
#8023 = CARTESIAN_POINT ( 'NONE',  ( -4.421511984667446784E-16, 3.660093687634854209, 1.660531772554310947 ) ) ;
#8024 = ORIENTED_EDGE ( 'NONE', *, *, #2988, .T. ) ;
#8025 = ORIENTED_EDGE ( 'NONE', *, *, #11330, .F. ) ;
#8027 = LINE ( 'NONE', #4641, #2320 ) ;
#8026 = VECTOR ( 'NONE', #6723, 1000.000000000000114 ) ;
#8028 = CARTESIAN_POINT ( 'NONE',  ( 642.5000000000001137, 160.0000000000000284, -210.0000059999999849 ) ) ;
#8030 = LINE ( 'NONE', #12534, #8259 ) ;
#8029 = AXIS2_PLACEMENT_3D ( 'NONE', #9435, #4936, #13637 ) ;
#8031 = ADVANCED_FACE ( 'NONE', ( #5048 ), #8124, .F. ) ;
#8032 = MECHANICAL_DESIGN_GEOMETRIC_PRESENTATION_REPRESENTATION (  '', ( #6154 ), #7093 ) ;
#8033 = DIRECTION ( 'NONE',  ( -0.000000000000000000, -0.000000000000000000, -1.000000000000000000 ) ) ;
#8034 = EDGE_CURVE ( 'NONE', #8972, #5634, #291, .T. ) ;
#8035 = CARTESIAN_POINT ( 'NONE',  ( 7.900000000000002132, 0.000000000000000000, 7.900000000000002132 ) ) ;
#8036 = CARTESIAN_POINT ( 'NONE',  ( 0.000000000000000000, 0.000000000000000000, 187.5000000000000000 ) ) ;
#8037 = VECTOR ( 'NONE', #9068, 1000.000000000000000 ) ;
#8038 = CARTESIAN_POINT ( 'NONE',  ( 610.0000000000001137, 227.4403065089106235, -184.8000000000000114 ) ) ;
#8039 = ORIENTED_EDGE ( 'NONE', *, *, #2288, .T. ) ;
#8040 = VECTOR ( 'NONE', #10369, 1000.000000000000000 ) ;
#8041 = CARTESIAN_POINT ( 'NONE',  ( 137.1540310085880776, 355.9707293956415697, -210.0000000000000000 ) ) ;
#8042 = PLANE ( 'NONE',  #872 ) ;
#8043 = DIRECTION ( 'NONE',  ( 0.03086419753086420623, -0.9995235871707959241, 0.000000000000000000 ) ) ;
#8044 = EDGE_LOOP ( 'NONE', ( #6714, #3730, #13627, #5713 ) ) ;
#8045 = CONICAL_SURFACE ( 'NONE', #1, 2.041999999999999815, 1.047197551196591858 ) ;
#8046 = CARTESIAN_POINT ( 'NONE',  ( 4.203833317240879275, 1.627343821129582979, -3.597273115243889929 ) ) ;
#8047 = ORIENTED_EDGE ( 'NONE', *, *, #3683, .F. ) ;
#8048 = EDGE_LOOP ( 'NONE', ( #4457, #5691, #7481, #1129 ) ) ;
#8049 = CARTESIAN_POINT ( 'NONE',  ( 4.211140560182196957, -2.431303136016555122, -3.745885042887436622 ) ) ;
#8050 = DIRECTION ( 'NONE',  ( 0.000000000000000000, 0.000000000000000000, 1.000000000000000000 ) ) ;
#8051 = CARTESIAN_POINT ( 'NONE',  ( 6.506987859255527695, -2.925375531177292210, 5.066899051217877314 ) ) ;
#8052 = AXIS2_PLACEMENT_3D ( 'NONE', #3583, #8881, #8071 ) ;
#8053 = DIRECTION ( 'NONE',  ( 0.9578262852211513190, -0.2873478855663453846, 0.000000000000000000 ) ) ;
#8054 = LINE ( 'NONE', #1185, #13852 ) ;
#8055 = EDGE_LOOP ( 'NONE', ( #11530, #8177 ) ) ;
#8056 = CARTESIAN_POINT ( 'NONE',  ( -4.000000000000000000, -7.806255641895631925E-15, -3.142992957459232350 ) ) ;
#8057 = DIRECTION ( 'NONE',  ( 0.000000000000000000, 0.000000000000000000, 1.000000000000000000 ) ) ;
#8058 = CARTESIAN_POINT ( 'NONE',  ( 0.000000000000000000, 0.000000000000000000, 0.000000000000000000 ) ) ;
#8059 = VECTOR ( 'NONE', #1251, 1000.000000000000114 ) ;
#8060 = DIRECTION ( 'NONE',  ( 0.000000000000000000, 0.000000000000000000, 1.000000000000000000 ) ) ;
#8061 = ORIENTED_EDGE ( 'NONE', *, *, #1395, .T. ) ;
#8062 = ORIENTED_EDGE ( 'NONE', *, *, #1312, .T. ) ;
#8063 = LINE ( 'NONE', #2379, #14084 ) ;
#8064 = CARTESIAN_POINT ( 'NONE',  ( 0.000000000000000000, 0.5192545390863916310, -1.000000000000000000 ) ) ;
#8065 = EDGE_CURVE ( 'NONE', #12523, #5769, #8743, .T. ) ;
#8066 = AXIS2_PLACEMENT_3D ( 'NONE', #4758, #3789, #2674 ) ;
#8067 = CARTESIAN_POINT ( 'NONE',  ( 9.498873539028489220E-16, -10.00000000000000000, -190.0000000000000000 ) ) ;
#8068 = CARTESIAN_POINT ( 'NONE',  ( 635.0000000000000000, 160.0000000000000284, -210.0000000000000000 ) ) ;
#8069 = ORIENTED_EDGE ( 'NONE', *, *, #14083, .F. ) ;
#8070 = ORIENTED_EDGE ( 'NONE', *, *, #11394, .T. ) ;
#8071 = DIRECTION ( 'NONE',  ( 1.000000000000000000, 0.000000000000000000, 0.000000000000000000 ) ) ;
#8072 = PLANE ( 'NONE',  #7784 ) ;
#8073 = CARTESIAN_POINT ( 'NONE',  ( -10.00000000000000000, 413.4403065089105667, 210.0000000000000000 ) ) ;
#8074 = LINE ( 'NONE', #4392, #12914 ) ;
#8075 = CARTESIAN_POINT ( 'NONE',  ( 0.000000000000000000, -3.464101615137757051, -1.999999999999996225 ) ) ;
#8076 = VERTEX_POINT ( 'NONE', #12855 ) ;
#8077 = FACE_OUTER_BOUND ( 'NONE', #1570, .T. ) ;
#8078 = ORIENTED_EDGE ( 'NONE', *, *, #10260, .T. ) ;
#8079 = EDGE_LOOP ( 'NONE', ( #14080, #1394, #1031, #565 ) ) ;
#8080 = CARTESIAN_POINT ( 'NONE',  ( 6.207519134556300777, 1.039264565629510528, -4.999999999999555023 ) ) ;
#8081 = EDGE_CURVE ( 'NONE', #9723, #4197, #2512, .T. ) ;
#8082 = ADVANCED_FACE ( 'NONE', ( #2814 ), #4759, .F. ) ;
#8083 = CARTESIAN_POINT ( 'NONE',  ( 629.0000000000000000, 166.0000000000000284, -187.5000000000000000 ) ) ;
#8084 = DIRECTION ( 'NONE',  ( 0.000000000000000000, -0.4999999999999993339, 0.8660254037844390407 ) ) ;
#8085 = EDGE_CURVE ( 'NONE', #10698, #9444, #13976, .T. ) ;
#8086 = VERTEX_POINT ( 'NONE', #2736 ) ;
#8087 = DIRECTION ( 'NONE',  ( 0.000000000000000000, 0.000000000000000000, 1.000000000000000000 ) ) ;
#8088 = PLANE ( 'NONE',  #11296 ) ;
#8090 = ADVANCED_FACE ( 'NONE', ( #522 ), #10345, .T. ) ;
#8089 = VECTOR ( 'NONE', #9035, 1000.000000000000114 ) ;
#8091 = LINE ( 'NONE', #10235, #2046 ) ;
#8092 = FACE_OUTER_BOUND ( 'NONE', #5082, .T. ) ;
#8093 = ORIENTED_EDGE ( 'NONE', *, *, #4583, .F. ) ;
#8094 = CARTESIAN_POINT ( 'NONE',  ( 6.367873360227555679, -2.886751345948120662, 4.999999999999999112 ) ) ;
#8095 = ORIENTED_EDGE ( 'NONE', *, *, #1748, .F. ) ;
#8096 = VERTEX_POINT ( 'NONE', #3791 ) ;
#8097 = CARTESIAN_POINT ( 'NONE',  ( 4.424031367840750129, -4.951337798339555007, -6.056431503347240231 ) ) ;
#8098 = LINE ( 'NONE', #12533, #13198 ) ;
#8099 = EDGE_CURVE ( 'NONE', #3368, #7099, #13751, .T. ) ;
#8100 = DIRECTION ( 'NONE',  ( -0.9578262852211513190, 0.2873478855663455511, -1.972152263052529951E-31 ) ) ;
#8101 = EDGE_CURVE ( 'NONE', #2217, #5202, #4826, .T. ) ;
#8102 = ORIENTED_EDGE ( 'NONE', *, *, #3203, .T. ) ;
#8103 = DIRECTION ( 'NONE',  ( 0.1305261922200524338, 0.9914448613738102711, 0.000000000000000000 ) ) ;
#8104 = EDGE_CURVE ( 'NONE', #3065, #8217, #1814, .T. ) ;
#8105 = CARTESIAN_POINT ( 'NONE',  ( 0.000000000000000000, 0.000000000000000000, -0.4621369752184044666 ) ) ;
#8106 = LINE ( 'NONE', #1088, #225 ) ;
#8107 = CARTESIAN_POINT ( 'NONE',  ( 8.451592086771722331E-13, 7.790254909845437226, -6.526045885145573600 ) ) ;
#8108 = ORIENTED_EDGE ( 'NONE', *, *, #8442, .F. ) ;
#8109 = CARTESIAN_POINT ( 'NONE',  ( -1.098735407079250326, -7.248058225758884809, -6.326622577870279152 ) ) ;
#8110 = FACE_OUTER_BOUND ( 'NONE', #13806, .T. ) ;
#8111 = ORIENTED_EDGE ( 'NONE', *, *, #12332, .F. ) ;
#8112 = CARTESIAN_POINT ( 'NONE',  ( 6.362382503762741948, -2.018850626433581041, 5.108861885121540602 ) ) ;
#8113 = ORIENTED_EDGE ( 'NONE', *, *, #4486, .F. ) ;
#8114 = ORIENTED_EDGE ( 'NONE', *, *, #6669, .F. ) ;
#8115 = CARTESIAN_POINT ( 'NONE',  ( 0.2259792476677715822, 7.636022678937395725, -6.470294263593361350 ) ) ;
#8116 = LINE ( 'NONE', #7086, #7525 ) ;
#8117 = DIRECTION ( 'NONE',  ( 0.9578262852211513190, -0.2873478855663455511, 0.000000000000000000 ) ) ;
#8118 = PRODUCT_DEFINITION_CONTEXT ( 'detailed design', #1508, 'design' ) ;
#8119 = DIRECTION ( 'NONE',  ( 1.000000000000000000, 0.000000000000000000, 0.000000000000000000 ) ) ;
#8120 = ORIENTED_EDGE ( 'NONE', *, *, #14580, .T. ) ;
#8121 = DIRECTION ( 'NONE',  ( -0.000000000000000000, -0.000000000000000000, -1.000000000000000000 ) ) ;
#8122 = DIRECTION ( 'NONE',  ( -0.000000000000000000, 0.000000000000000000, 1.000000000000000000 ) ) ;
#8123 = DIRECTION ( 'NONE',  ( 0.000000000000000000, 0.000000000000000000, 1.000000000000000000 ) ) ;
#8124 = PLANE ( 'NONE',  #9922 ) ;
#8125 = ORIENTED_EDGE ( 'NONE', *, *, #4783, .F. ) ;
#8126 = ORIENTED_EDGE ( 'NONE', *, *, #1079, .F. ) ;
#8127 = CARTESIAN_POINT ( 'NONE',  ( 635.9817477042469136, 152.4999999999999716, 210.0000119999999981 ) ) ;
#8128 = LINE ( 'NONE', #3931, #12998 ) ;
#8129 = CARTESIAN_POINT ( 'NONE',  ( 6.541171661047875396, 2.934678558896536504, 5.142480235691129664 ) ) ;
#8130 = ORIENTED_EDGE ( 'NONE', *, *, #9009, .F. ) ;
#8131 = EDGE_LOOP ( 'NONE', ( #11128, #8570, #13589, #8422 ) ) ;
#8132 = CARTESIAN_POINT ( 'NONE',  ( 6.518095160332176619, -2.933089652807386649, -5.080260301816938551 ) ) ;
#8133 = ADVANCED_FACE ( 'NONE', ( #4893, #9389 ), #8275, .F. ) ;
#8134 = CARTESIAN_POINT ( 'NONE',  ( 0.5620262070071402327, -7.564407249984300918, -6.443844059477449093 ) ) ;
#8135 = EDGE_CURVE ( 'NONE', #12947, #9303, #5261, .T. ) ;
#8136 = CARTESIAN_POINT ( 'NONE',  ( 6.481779955677546390, 5.820445026626438256, 9.200230307558180419E-16 ) ) ;
#8137 = DIRECTION ( 'NONE',  ( -1.000000000000000000, 0.000000000000000000, 0.000000000000000000 ) ) ;
#8138 = CARTESIAN_POINT ( 'NONE',  ( -2.263183130831070589, 6.566419505188274996, -6.208110906918258287 ) ) ;
#8139 = VERTEX_POINT ( 'NONE', #6356 ) ;
#8140 = CARTESIAN_POINT ( 'NONE',  ( -4.000000000000003553, 2.309401076758496263, -3.504269196027868905 ) ) ;
#8141 = EDGE_LOOP ( 'NONE', ( #12341, #4180 ) ) ;
#8142 = VERTEX_POINT ( 'NONE', #10714 ) ;
#8143 = CARTESIAN_POINT ( 'NONE',  ( 33.05499999999999972, 0.000000000000000000, 0.000000000000000000 ) ) ;
#8144 = DIRECTION ( 'NONE',  ( 0.000000000000000000, 0.000000000000000000, 1.000000000000000000 ) ) ;
#8145 = LINE ( 'NONE', #5868, #10640 ) ;
#8146 = ORIENTED_EDGE ( 'NONE', *, *, #5951, .F. ) ;
#8147 = LINE ( 'NONE', #12656, #4770 ) ;
#8148 = ADVANCED_FACE ( 'NONE', ( #14189 ), #8497, .F. ) ;
#8149 = CARTESIAN_POINT ( 'NONE',  ( 3.700000000000000178, 0.000000000000000000, 0.000000000000000000 ) ) ;
#8150 = ADVANCED_FACE ( 'NONE', ( #9823 ), #6276, .F. ) ;
#8151 = CARTESIAN_POINT ( 'NONE',  ( -2.742827927723112236, -3.035229711105190464, -3.433252694550595230 ) ) ;
#8152 = PRESENTATION_STYLE_ASSIGNMENT (( #95 ) ) ;
#8153 = VERTEX_POINT ( 'NONE', #10863 ) ;
#8154 = CARTESIAN_POINT ( 'NONE',  ( 635.0000000000000000, 160.0000000000000284, -187.5000000000000000 ) ) ;
#8155 =( BOUNDED_SURFACE ( )  B_SPLINE_SURFACE ( 3, 2, ( 
 ( #11925, #3767, #8396 ),
 ( #6037, #14025, #10541 ),
 ( #415, #8327, #8474 ),
 ( #13953, #10623, #570 ),
 ( #5093, #3846, #10759 ),
 ( #637, #5161, #10696 ) ),
 .UNSPECIFIED., .F., .F., .T. ) 
 B_SPLINE_SURFACE_WITH_KNOTS ( ( 4, 2, 4 ),
 ( 3, 3 ),
 ( 0.02027752710269158445, 0.02273781595091097299, 0.02519810479913036153 ),
 ( 0.000000000000000000, 1.000000000000000000 ),
 .UNSPECIFIED. ) 
 GEOMETRIC_REPRESENTATION_ITEM ( )  RATIONAL_B_SPLINE_SURFACE ( (
 ( 1.000000000000000000, 0.8047781431712808242, 1.000000000000000000),
 ( 1.000000000000000000, 0.8123773247083928561, 1.000000000000000000),
 ( 1.000000000000000000, 0.8190670192154906326, 1.000000000000000000),
 ( 1.000000000000000000, 0.8192353552912178261, 1.000000000000000000),
 ( 1.000000000000000000, 0.8126132098226825917, 1.000000000000000000),
 ( 1.000000000000000000, 0.8047712465856394770, 1.000000000000000000) ) ) 
 REPRESENTATION_ITEM ( '' )  SURFACE ( )  );
#8156 = VERTEX_POINT ( 'NONE', #9760 ) ;
#8157 = EDGE_CURVE ( 'NONE', #12715, #2075, #7398, .T. ) ;
#8158 = ORIENTED_EDGE ( 'NONE', *, *, #4607, .T. ) ;
#8159 = CARTESIAN_POINT ( 'NONE',  ( 610.0000000000000000, 175.0000000000000568, -190.0000000000000000 ) ) ;
#8160 = PRODUCT ( 'sliding track', 'sliding track', '', ( #1171 ) ) ;
#8161 = CARTESIAN_POINT ( 'NONE',  ( -4.000000000000000000, 0.000000000000000000, 0.000000000000000000 ) ) ;
#8162 = FACE_OUTER_BOUND ( 'NONE', #4317, .T. ) ;
#8163 = VERTEX_POINT ( 'NONE', #11884 ) ;
#8164 = LINE ( 'NONE', #8321, #5232 ) ;
#8165 = EDGE_CURVE ( 'NONE', #9542, #13868, #3036, .T. ) ;
#8166 = CIRCLE ( 'NONE', #5586, 4.799999999999999822 ) ;
#8167 = DIRECTION ( 'NONE',  ( 0.000000000000000000, 0.000000000000000000, 1.000000000000000000 ) ) ;
#8168 = CARTESIAN_POINT ( 'NONE',  ( -6.815830331203684089, 0.6610623347507950109, -6.171384342982605631 ) ) ;
#8169 = DIRECTION ( 'NONE',  ( -0.000000000000000000, -0.000000000000000000, -1.000000000000000000 ) ) ;
#8170 = ORIENTED_EDGE ( 'NONE', *, *, #1243, .F. ) ;
#8171 = FACE_OUTER_BOUND ( 'NONE', #4274, .T. ) ;
#8172 = LINE ( 'NONE', #12683, #14082 ) ;
#8173 = ORIENTED_EDGE ( 'NONE', *, *, #10784, .F. ) ;
#8174 = EDGE_CURVE ( 'NONE', #5554, #11494, #4266, .T. ) ;
#8175 = CARTESIAN_POINT ( 'NONE',  ( 6.092439126518621073, 1.005559546149547678, 4.999999999999999112 ) ) ;
#8176 = ORIENTED_EDGE ( 'NONE', *, *, #5394, .T. ) ;
#8177 = ORIENTED_EDGE ( 'NONE', *, *, #10784, .T. ) ;
#8178 = SURFACE_SIDE_STYLE ('',( #11649 ) ) ;
#8179 = CARTESIAN_POINT ( 'NONE',  ( -0.8808064505788995024, 6.997019658119450369, -5.875704392893736916 ) ) ;
#8180 = AXIS2_PLACEMENT_3D ( 'NONE', #4132, #6261, #638 ) ;
#8181 = EDGE_CURVE ( 'NONE', #8669, #5128, #5901, .T. ) ;
#8183 = CARTESIAN_POINT ( 'NONE',  ( 2.000000000000008882, 3.464101615137749945, 0.000000000000000000 ) ) ;
#8182 = AXIS2_PLACEMENT_3D ( 'NONE', #3429, #4463, #7869 ) ;
#8184 = PRODUCT_DEFINITION ( 'UNKNOWN', '', #10199, #5040 ) ;
#8185 = CARTESIAN_POINT ( 'NONE',  ( 0.3572655899081595976, 2.309401076758508253, 3.999999999999993339 ) ) ;
#8186 = DIRECTION ( 'NONE',  ( 4.427295178148650474E-30, -1.328188553444596088E-30, 1.000000000000000000 ) ) ;
#8187 = ORIENTED_EDGE ( 'NONE', *, *, #281, .F. ) ;
#8188=STYLED_ITEM('',(#14688),#2557);
#8189 = CIRCLE ( 'NONE', #13624, 7.000000000000006217 ) ;
#8190 = CARTESIAN_POINT ( 'NONE',  ( 703.1581845006096501, 166.2926764603917036, 177.6000000000001648 ) ) ;
#8191 = DIRECTION ( 'NONE',  ( 1.003269780210927276E-15, 3.344232600703091053E-15, 1.000000000000000000 ) ) ;
#8192 = CARTESIAN_POINT ( 'NONE',  ( 446.3084422793565409, 264.0194060144110608, 215.0000000000000000 ) ) ;
#8193 = CARTESIAN_POINT ( 'NONE',  ( 6.533910050139694725, 2.950514251728050485, 5.110440592449069896 ) ) ;
#8194 = ORIENTED_EDGE ( 'NONE', *, *, #1471, .T. ) ;
#8195 = ORIENTED_EDGE ( 'NONE', *, *, #13842, .T. ) ;
#8196 = B_SPLINE_CURVE_WITH_KNOTS ( 'NONE', 3,
 ( #11244, #1056, #13472, #5565, #10065, #13543 ),
 .UNSPECIFIED., .F., .F.,
 ( 4, 2, 4 ),
 ( 0.002365888236227977302, 0.003551327329835078910, 0.004736766423442180518 ),
 .UNSPECIFIED. ) ;
#8197 = CARTESIAN_POINT ( 'NONE',  ( 3.309651814758564736, -5.455921364805393026, 0.000000000000000000 ) ) ;
#8198 = DIRECTION ( 'NONE',  ( 1.000000000000000000, 0.000000000000000000, 0.000000000000000000 ) ) ;
#8199 =( REPRESENTATION_RELATIONSHIP ('NONE','NONE', #2822, #6779 ) REPRESENTATION_RELATIONSHIP_WITH_TRANSFORMATION ( #7430 )SHAPE_REPRESENTATION_RELATIONSHIP( ) );
#8200 = PRODUCT_RELATED_PRODUCT_CATEGORY ( 'part', '', ( #6049 ) ) ;
#8201 = CARTESIAN_POINT ( 'NONE',  ( 6.204460410672266946, 4.828986228461177532, 1.635950503255240607 ) ) ;
#8202 = AXIS2_PLACEMENT_3D ( 'NONE', #4757, #3642, #8122 ) ;
#8203 = AXIS2_PLACEMENT_3D ( 'NONE', #5535, #5470, #2960 ) ;
#8204 = ORIENTED_EDGE ( 'NONE', *, *, #9413, .F. ) ;
#8205 = EDGE_CURVE ( 'NONE', #1376, #3502, #7322, .T. ) ;
#8206 = CARTESIAN_POINT ( 'NONE',  ( 446.3084422793565409, 264.0194060144110608, 190.0000000000000000 ) ) ;
#8207 = CARTESIAN_POINT ( 'NONE',  ( -6.259644161404859044E-16, -4.618802153517026277, -3.504271511727133248 ) ) ;
#8208 = DIRECTION ( 'NONE',  ( -0.000000000000000000, 0.000000000000000000, 1.000000000000000000 ) ) ;
#8209 = EDGE_CURVE ( 'NONE', #6705, #14270, #14259, .T. ) ;
#8210 = CARTESIAN_POINT ( 'NONE',  ( 5.200000000000002842, 0.000000000000000000, 0.000000000000000000 ) ) ;
#8211 = CARTESIAN_POINT ( 'NONE',  ( 610.0000000000000000, 145.0000000000000568, 210.0000000000000000 ) ) ;
#8212 =( LENGTH_UNIT ( ) NAMED_UNIT ( * ) SI_UNIT ( .MILLI., .METRE. ) );
#8213 = ORIENTED_EDGE ( 'NONE', *, *, #9717, .F. ) ;
#8214 = VECTOR ( 'NONE', #11388, 1000.000000000000000 ) ;
#8215 = CARTESIAN_POINT ( 'NONE',  ( 1.360585162435110629, -4.061296242128317857, -3.505054077164905024 ) ) ;
#8216 = AXIS2_PLACEMENT_3D ( 'NONE', #7323, #14116, #1853 ) ;
#8217 = VERTEX_POINT ( 'NONE', #10778 ) ;
#8218 = EDGE_LOOP ( 'NONE', ( #10886, #928, #10540, #8740 ) ) ;
#8219 = CARTESIAN_POINT ( 'NONE',  ( 8.542937654374687995, 0.000000000000000000, -6.800000000000000711 ) ) ;
#8220 = TOROIDAL_SURFACE ( 'NONE', #8934, 7.399999999999999467, 0.1000000000000000472 ) ;
#8221 = EDGE_CURVE ( 'NONE', #10951, #1218, #2962, .T. ) ;
#8222 = CARTESIAN_POINT ( 'NONE',  ( 7.336184427528458230, 9.926022037524705097E-16, 8.105212085995399107 ) ) ;
#8223 = CARTESIAN_POINT ( 'NONE',  ( 2.999999999999999112, -3.464101615137750834, 2.000000000000007994 ) ) ;
#8224 = AXIS2_PLACEMENT_3D ( 'NONE', #2800, #2726, #6342 ) ;
#8225 = CARTESIAN_POINT ( 'NONE',  ( 145.1678582058265476, 408.6511750828048548, -190.0000000000000000 ) ) ;
#8226 = VECTOR ( 'NONE', #4407, 1000.000000000000000 ) ;
#8227 = ORIENTED_EDGE ( 'NONE', *, *, #1576, .T. ) ;
#8228 = CARTESIAN_POINT ( 'NONE',  ( 2.595115354961440524, -7.673029147243177306, 0.000000000000000000 ) ) ;
#8229 = DIRECTION ( 'NONE',  ( 0.000000000000000000, -1.000000000000000000, 0.000000000000000000 ) ) ;
#8230 = DIRECTION ( 'NONE',  ( 1.000000000000000000, 0.000000000000000000, 0.000000000000000000 ) ) ;
#8231 = DIRECTION ( 'NONE',  ( 1.000000000000000000, 0.000000000000000000, 0.000000000000000000 ) ) ;
#8232 = FILL_AREA_STYLE ('',( #9423 ) ) ;
#8233 = VERTEX_POINT ( 'NONE', #738 ) ;
#8234 = VECTOR ( 'NONE', #6319, 1000.000000000000000 ) ;
#8235 = FACE_BOUND ( 'NONE', #4400, .T. ) ;
#8236 = ORIENTED_EDGE ( 'NONE', *, *, #8437, .T. ) ;
#8237 = VECTOR ( 'NONE', #14295, 1000.000000000000000 ) ;
#8238 = CIRCLE ( 'NONE', #11305, 0.1000000000000002554 ) ;
#8239 = DIRECTION ( 'NONE',  ( 1.000000000000000000, 0.000000000000000000, 0.000000000000000000 ) ) ;
#8240 = EDGE_CURVE ( 'NONE', #9997, #9391, #11815, .T. ) ;
#8241 = DIRECTION ( 'NONE',  ( 0.000000000000000000, -1.224646799147353454E-16, 1.000000000000000000 ) ) ;
#8242 = CARTESIAN_POINT ( 'NONE',  ( 4.000000000000000000, 2.309401076758497151, -3.433295621305379353 ) ) ;
#8243 = ORIENTED_EDGE ( 'NONE', *, *, #11797, .T. ) ;
#8244 = CARTESIAN_POINT ( 'NONE',  ( 609.9289135522120660, 190.4185930515760958, 190.0000000000000284 ) ) ;
#8245 = AXIS2_PLACEMENT_3D ( 'NONE', #4403, #14451, #13267 ) ;
#8246 = DIRECTION ( 'NONE',  ( 0.000000000000000000, 0.000000000000000000, -1.000000000000000000 ) ) ;
#8247 = CARTESIAN_POINT ( 'NONE',  ( -3.965067105215785097E-15, -4.207632145829741432, 2.712167343862823099 ) ) ;
#8248 = CARTESIAN_POINT ( 'NONE',  ( 4.175002511812151873, 2.208363329454889445, -3.469254087858244073 ) ) ;
#8249 = ORIENTED_EDGE ( 'NONE', *, *, #11979, .T. ) ;
#8250 = CARTESIAN_POINT ( 'NONE',  ( -10.00000000000000000, 0.000000000000000000, 190.0000000000000000 ) ) ;
#8251 = ORIENTED_EDGE ( 'NONE', *, *, #12653, .T. ) ;
#8252 = AXIS2_PLACEMENT_3D ( 'NONE', #6044, #4744, #12690 ) ;
#8253 = AXIS2_PLACEMENT_3D ( 'NONE', #2375, #4447, #7980 ) ;
#8254 = CARTESIAN_POINT ( 'NONE',  ( 6.506891485183659896, -2.992470280394939675, 5.000000000000000000 ) ) ;
#8255 = VERTEX_POINT ( 'NONE', #14107 ) ;
#8256 = VERTEX_POINT ( 'NONE', #12103 ) ;
#8257 = CARTESIAN_POINT ( 'NONE',  ( 446.3084422793565409, 264.0194060144110608, 190.0000000000000000 ) ) ;
#8258 = EDGE_CURVE ( 'NONE', #14073, #14292, #4496, .T. ) ;
#8259 = VECTOR ( 'NONE', #3838, 1000.000000000000114 ) ;
#8260 = AXIS2_PLACEMENT_3D ( 'NONE', #8036, #11361, #12450 ) ;
#8261 = CARTESIAN_POINT ( 'NONE',  ( 6.534224484704351354, -2.950930484791602471, 5.111161529262889580 ) ) ;
#8262 = EDGE_CURVE ( 'NONE', #6382, #5721, #10934, .T. ) ;
#8263 = CARTESIAN_POINT ( 'NONE',  ( -4.024497503033714452, -2.323544716729502468, -3.572167766733752803 ) ) ;
#8264 = CONICAL_SURFACE ( 'NONE', #9932, 4.000000000000000000, 0.8911886515913786111 ) ;
#8265 = EDGE_CURVE ( 'NONE', #1716, #4246, #806, .T. ) ;
#8266 = UNCERTAINTY_MEASURE_WITH_UNIT (LENGTH_MEASURE( 1.000000000000000082E-05 ), #13389, 'distance_accuracy_value', 'NONE');
#8267 = CARTESIAN_POINT ( 'NONE',  ( 1.500000000000001332, 0.000000000000000000, 0.000000000000000000 ) ) ;
#8268 = VERTEX_POINT ( 'NONE', #5178 ) ;
#8269 = AXIS2_PLACEMENT_3D ( 'NONE', #2247, #11259, #6625 ) ;
#8270 = EDGE_CURVE ( 'NONE', #10585, #8972, #13144, .T. ) ;
#8271 = CARTESIAN_POINT ( 'NONE',  ( 0.1983443223721576831, 5.300482436767277150, 0.8192951148925904370 ) ) ;
#8272 = CARTESIAN_POINT ( 'NONE',  ( 8.500000000000000000, 2.886751345948122882, -5.000000000000000000 ) ) ;
#8273 = DIRECTION ( 'NONE',  ( -1.000000000000000000, 0.000000000000000000, 0.000000000000000000 ) ) ;
#8274 = EDGE_CURVE ( 'NONE', #9802, #809, #6505, .T. ) ;
#8275 = PLANE ( 'NONE',  #3560 ) ;
#8276 = ORIENTED_EDGE ( 'NONE', *, *, #8287, .F. ) ;
#8277 = EDGE_LOOP ( 'NONE', ( #1607, #3974, #14364, #14558 ) ) ;
#8278 = AXIS2_PLACEMENT_3D ( 'NONE', #3685, #13726, #8103 ) ;
#8279 = DIRECTION ( 'NONE',  ( -1.000000000000000000, -0.000000000000000000, -0.000000000000000000 ) ) ;
#8280 = DIRECTION ( 'NONE',  ( -0.000000000000000000, 0.8660254037844387076, 0.5000000000000001110 ) ) ;
#8281 = CIRCLE ( 'NONE', #7545, 2.499999999999946709 ) ;
#8282 = DIRECTION ( 'NONE',  ( 1.000000000000000000, 9.498873539028489960E-17, 0.000000000000000000 ) ) ;
#8283 = STYLED_ITEM ( 'NONE', ( #2305 ), #4208 ) ;
#8284 = DIRECTION ( 'NONE',  ( -0.000000000000000000, -0.000000000000000000, -1.000000000000000000 ) ) ;
#8285 = EDGE_CURVE ( 'NONE', #483, #9255, #11554, .T. ) ;
#8286 = VERTEX_POINT ( 'NONE', #3333 ) ;
#8287 = EDGE_CURVE ( 'NONE', #4931, #6458, #13354, .T. ) ;
#8288 = DIRECTION ( 'NONE',  ( 0.000000000000000000, -1.000000000000000000, 0.000000000000000000 ) ) ;
#8289 = CARTESIAN_POINT ( 'NONE',  ( 610.6294623944595514, 188.6821150189054777, -185.3758453455904771 ) ) ;
#8290 = DIRECTION ( 'NONE',  ( -0.2873478855663453846, -0.9578262852211513190, -0.000000000000000000 ) ) ;
#8291 = EDGE_CURVE ( 'NONE', #1120, #12176, #13777, .T. ) ;
#8292 = FACE_BOUND ( 'NONE', #5355, .T. ) ;
#8293 = DIRECTION ( 'NONE',  ( 1.000000000000000000, 0.000000000000000000, -0.000000000000000000 ) ) ;
#8294 = PRODUCT_DEFINITION_SHAPE ( 'NONE', 'NONE',  #14621 ) ;
#8295 =( REPRESENTATION_RELATIONSHIP ('NONE','NONE', #2822, #1873 ) REPRESENTATION_RELATIONSHIP_WITH_TRANSFORMATION ( #3182 )SHAPE_REPRESENTATION_RELATIONSHIP( ) );
#8296 = ORIENTED_EDGE ( 'NONE', *, *, #10156, .T. ) ;
#8297 = DIRECTION ( 'NONE',  ( 0.000000000000000000, 0.000000000000000000, -1.000000000000000000 ) ) ;
#8298 = ORIENTED_EDGE ( 'NONE', *, *, #7901, .T. ) ;
#8299 = EDGE_LOOP ( 'NONE', ( #4491, #8367, #3432, #9472 ) ) ;
#8300 = DIRECTION ( 'NONE',  ( -0.000000000000000000, -0.000000000000000000, -1.000000000000000000 ) ) ;
#8301 = CIRCLE ( 'NONE', #11372, 0.7500000000000000000 ) ;
#8302 = CARTESIAN_POINT ( 'NONE',  ( -10.00000000000000000, 371.6790804732683569, 190.0000000000000000 ) ) ;
#8303 = CARTESIAN_POINT ( 'NONE',  ( 7.336184427528458230, 0.000000000000000000, 0.000000000000000000 ) ) ;
#8304 = FACE_OUTER_BOUND ( 'NONE', #5395, .T. ) ;
#8305 = PRODUCT_DEFINITION_FORMATION_WITH_SPECIFIED_SOURCE ( 'ANY', '', #9107, .NOT_KNOWN. ) ;
#8306 = ORIENTED_EDGE ( 'NONE', *, *, #7825, .F. ) ;
#8307 = LINE ( 'NONE', #3893, #11119 ) ;
#8308 = CYLINDRICAL_SURFACE ( 'NONE', #456, 8.099999999999999645 ) ;
#8309 = DIRECTION ( 'NONE',  ( 0.000000000000000000, 0.000000000000000000, -1.000000000000000000 ) ) ;
#8310 = DIRECTION ( 'NONE',  ( 0.000000000000000000, 0.000000000000000000, 1.000000000000000000 ) ) ;
#8311 = SURFACE_SIDE_STYLE ('',( #2853 ) ) ;
#8312 = VECTOR ( 'NONE', #10301, 1000.000000000000000 ) ;
#8313 = ORIENTED_EDGE ( 'NONE', *, *, #11654, .F. ) ;
#8314 = DIRECTION ( 'NONE',  ( 1.000000000000000000, 0.000000000000000000, 0.000000000000000000 ) ) ;
#8315 = ORIENTED_EDGE ( 'NONE', *, *, #849, .F. ) ;
#8316 = FACE_OUTER_BOUND ( 'NONE', #5372, .T. ) ;
#8317 = CARTESIAN_POINT ( 'NONE',  ( 1.500000000000001332, 0.000000000000000000, -7.399999999999999467 ) ) ;
#8318 = PRESENTATION_LAYER_ASSIGNMENT (  '', '', ( #51 ) ) ;
#8319 = PLANE ( 'NONE',  #3564 ) ;
#8320 = ORIENTED_EDGE ( 'NONE', *, *, #10968, .T. ) ;
#8321 = CARTESIAN_POINT ( 'NONE',  ( -3.309651814758565180, -5.455921364805393026, 0.000000000000000000 ) ) ;
#8322 = DIRECTION ( 'NONE',  ( 0.000000000000000000, 1.000000000000000000, 0.000000000000000000 ) ) ;
#8323 = CARTESIAN_POINT ( 'NONE',  ( 43.50000000000000711, 0.000000000000000000, 3.309499999999999886 ) ) ;
#8324 = LINE ( 'NONE', #3689, #3272 ) ;
#8325 = EDGE_CURVE ( 'NONE', #6439, #5548, #3082, .T. ) ;
#8326 = VERTEX_POINT ( 'NONE', #53 ) ;
#8327 = CARTESIAN_POINT ( 'NONE',  ( -4.000000000000000000, 0.8576368993457507139, -3.433240632782198709 ) ) ;
#8328 = LINE ( 'NONE', #12838, #5131 ) ;
#8329 = ORIENTED_EDGE ( 'NONE', *, *, #8917, .F. ) ;
#8330 = PLANE ( 'NONE',  #10159 ) ;
#8331 = ORIENTED_EDGE ( 'NONE', *, *, #12361, .F. ) ;
#8332 = ORIENTED_EDGE ( 'NONE', *, *, #10606, .F. ) ;
#8333 = CARTESIAN_POINT ( 'NONE',  ( 6.746887896522321348, -3.895317543249584347, -6.526184258131189075 ) ) ;
#8334 = B_SPLINE_CURVE_WITH_KNOTS ( 'NONE', 3,
 ( #1401, #346, #11583, #9236 ),
 .UNSPECIFIED., .F., .F.,
 ( 4, 4 ),
 ( 2.380737581620950413E-07, 0.002336974151641552089 ),
 .UNSPECIFIED. ) ;
#8335 = DIRECTION ( 'NONE',  ( -1.000000000000000000, 0.000000000000000000, 0.000000000000000000 ) ) ;
#8336 = LINE ( 'NONE', #2456, #4500 ) ;
#8337 = CARTESIAN_POINT ( 'NONE',  ( 455.5035746174796714, 294.6698471414878782, -187.0000000000000568 ) ) ;
#8338 = CARTESIAN_POINT ( 'NONE',  ( -8.505790995055004799, 418.4210031920606525, 190.0000000000000000 ) ) ;
#8339 = ADVANCED_FACE ( 'NONE', ( #4589 ), #12460, .F. ) ;
#8340 = ORIENTED_EDGE ( 'NONE', *, *, #14608, .F. ) ;
#8341 = B_SPLINE_CURVE_WITH_KNOTS ( 'NONE', 3,
 ( #12405, #1113, #6804, #7983, #12343, #13755 ),
 .UNSPECIFIED., .F., .F.,
 ( 4, 2, 4 ),
 ( 0.002452478801916361129, 0.003676905084148001344, 0.004901331366379641126 ),
 .UNSPECIFIED. ) ;
#8342 = LINE ( 'NONE', #7392, #6097 ) ;
#8343 = CARTESIAN_POINT ( 'NONE',  ( 6.500000000000000888, 0.000000000000000000, 0.000000000000000000 ) ) ;
#8344 = DIRECTION ( 'NONE',  ( -0.9945454910858376740, -0.1043037207429823865, 0.000000000000000000 ) ) ;
#8345 = ADVANCED_FACE ( 'NONE', ( #952 ), #6718, .T. ) ;
#8346 = CARTESIAN_POINT ( 'NONE',  ( 112.9652219749295341, 376.5507399164317803, -210.0000000000000000 ) ) ;
#8347 = VECTOR ( 'NONE', #12610, 1000.000000000000000 ) ;
#8348 = ORIENTED_EDGE ( 'NONE', *, *, #8205, .T. ) ;
#8349 = ORIENTED_EDGE ( 'NONE', *, *, #8165, .F. ) ;
#8350 = DIRECTION ( 'NONE',  ( 1.000000000000000000, 0.000000000000000000, 0.000000000000000000 ) ) ;
#8351 = DIRECTION ( 'NONE',  ( -1.000000000000000000, 0.000000000000000000, 0.000000000000000000 ) ) ;
#8352 = EDGE_CURVE ( 'NONE', #2860, #5297, #10787, .T. ) ;
#8353 = DIRECTION ( 'NONE',  ( 0.000000000000000000, 0.000000000000000000, -1.000000000000000000 ) ) ;
#8354 = ADVANCED_FACE ( 'NONE', ( #1261 ), #11147, .T. ) ;
#8355 = CARTESIAN_POINT ( 'NONE',  ( 632.5000000000001137, 160.0000000000000284, -217.5000000000000284 ) ) ;
#8356 = ORIENTED_EDGE ( 'NONE', *, *, #2027, .T. ) ;
#8357 = AXIS2_PLACEMENT_3D ( 'NONE', #10103, #4732, #10028 ) ;
#8358 = CARTESIAN_POINT ( 'NONE',  ( 0.000000000000000000, 0.000000000000000000, 0.000000000000000000 ) ) ;
#8359 = CARTESIAN_POINT ( 'NONE',  ( 6.534838248920899595, -2.951765777552421532, -5.112608298763837489 ) ) ;
#8360 = CARTESIAN_POINT ( 'NONE',  ( 2.500000000000000000, 0.000000000000000000, 0.000000000000000000 ) ) ;
#8361 = CARTESIAN_POINT ( 'NONE',  ( 5.200000000000002842, 0.000000000000000000, 2.500000000000000444 ) ) ;
#8362 = DIRECTION ( 'NONE',  ( -0.000000000000000000, 0.8660254037844392627, 0.4999999999999990008 ) ) ;
#8363 = CARTESIAN_POINT ( 'NONE',  ( 142.4540310085880606, 355.9707293956415697, 190.0000000000000000 ) ) ;
#8364 = ORIENTED_EDGE ( 'NONE', *, *, #3902, .T. ) ;
#8365 = DIRECTION ( 'NONE',  ( -0.000000000000000000, -0.000000000000000000, 1.000000000000000000 ) ) ;
#8366 = EDGE_LOOP ( 'NONE', ( #965, #154, #14125, #12886 ) ) ;
#8367 = ORIENTED_EDGE ( 'NONE', *, *, #2427, .T. ) ;
#8368 = LINE ( 'NONE', #9340, #491 ) ;
#8369 = ADVANCED_FACE ( 'NONE', ( #4515, #4655 ), #2357, .F. ) ;
#8370 = B_SPLINE_CURVE_WITH_KNOTS ( 'NONE', 3,
 ( #12367, #3303, #2252, #5799, #10380, #10300, #13407, #9057 ),
 .UNSPECIFIED., .F., .F.,
 ( 4, 2, 2, 4 ),
 ( 2.459764730912720885E-07, 0.001920659145285728234, 0.002880865729692047052, 0.003841072314098365435 ),
 .UNSPECIFIED. ) ;
#8371 = B_SPLINE_CURVE_WITH_KNOTS ( 'NONE', 3,
 ( #8359, #5850, #2746, #3806, #9328, #8132, #7253, #1565, #2687, #7183, #9485, #11740, #6156, #11673, #9553, #3936 ),
 .UNSPECIFIED., .F., .F.,
 ( 4, 3, 3, 3, 3, 4 ),
 ( -2.669610558405276678E-06, 4.235164736271501695E-22, 5.703179328867178207E-05, 0.0001157653700801148554, 0.0001686517580788998878, 0.0002219032271218163014 ),
 .UNSPECIFIED. ) ;
#8372 = EDGE_CURVE ( 'NONE', #4002, #3163, #7078, .T. ) ;
#8373 = CARTESIAN_POINT ( 'NONE',  ( 0.000000000000000000, 0.000000000000000000, -1.000000000000000000 ) ) ;
#8374 = PRODUCT_DEFINITION ( 'UNKNOWN', '', #6887, #4288 ) ;
#8375 = CARTESIAN_POINT ( 'NONE',  ( 628.0000000000000000, 152.9999999999999147, -233.5000000000000000 ) ) ;
#8376 = CARTESIAN_POINT ( 'NONE',  ( 6.500000000000000000, 3.752776749732563921, -6.064240316920399110 ) ) ;
#8377 = VERTEX_POINT ( 'NONE', #116 ) ;
#8378 = DIRECTION ( 'NONE',  ( -0.000000000000000000, -0.000000000000000000, -1.000000000000000000 ) ) ;
#8379 = CARTESIAN_POINT ( 'NONE',  ( 1.500000000000000888, 6.245698675651501825E-16, 5.100000000000000533 ) ) ;
#8380 = DIRECTION ( 'NONE',  ( 0.2873478855663502141, 0.9578262852211498757, -4.382459307730876264E-15 ) ) ;
#8381 = LINE ( 'NONE', #4858, #4323 ) ;
#8382 = ORIENTED_EDGE ( 'NONE', *, *, #9646, .F. ) ;
#8383 = DIRECTION ( 'NONE',  ( -0.000000000000000000, -0.000000000000000000, 1.000000000000000000 ) ) ;
#8384 = CARTESIAN_POINT ( 'NONE',  ( 636.7009106935324780, 155.5114698605638637, -210.0000000000000000 ) ) ;
#8385 = ORIENTED_EDGE ( 'NONE', *, *, #5949, .T. ) ;
#8386 = FACE_BOUND ( 'NONE', #2402, .T. ) ;
#8387 = DIRECTION ( 'NONE',  ( -1.000000000000000000, -0.000000000000000000, -0.000000000000000000 ) ) ;
#8388 = CARTESIAN_POINT ( 'NONE',  ( 629.0000000000000000, 166.0000000000000284, 187.5000000000000000 ) ) ;
#8389 = EDGE_LOOP ( 'NONE', ( #14213, #2093 ) ) ;
#8390 = CARTESIAN_POINT ( 'NONE',  ( 609.7898554267394502, 185.8834251265051307, 186.1610889986683048 ) ) ;
#8391 = CARTESIAN_POINT ( 'NONE',  ( 610.8620436566991430, 188.5525593289319488, -184.8000000000000398 ) ) ;
#8392 = DIRECTION ( 'NONE',  ( 0.000000000000000000, 0.000000000000000000, 1.000000000000000000 ) ) ;
#8393 = CARTESIAN_POINT ( 'NONE',  ( -1.101549646961929599E-15, 7.550813340387652950, -6.286444963328673197 ) ) ;
#8394 = ORIENTED_EDGE ( 'NONE', *, *, #9171, .T. ) ;
#8395 = ADVANCED_FACE ( 'NONE', ( #5606 ), #4366, .F. ) ;
#8396 = CARTESIAN_POINT ( 'NONE',  ( -4.211399284164270895, 2.459729995988205964, -3.751162237960538715 ) ) ;
#8397 =( LENGTH_UNIT ( ) NAMED_UNIT ( * ) SI_UNIT ( .MILLI., .METRE. ) );
#8398 = ORIENTED_EDGE ( 'NONE', *, *, #12194, .T. ) ;
#8399 = EDGE_LOOP ( 'NONE', ( #10240, #2458, #7879, #3109, #215, #5791, #10762 ) ) ;
#8400 = CARTESIAN_POINT ( 'NONE',  ( 636.9746078850427011, 155.6249658629529620, 210.0000000000000000 ) ) ;
#8401 = CARTESIAN_POINT ( 'NONE',  ( 4.639619758716984954, -4.826867782832383824, -0.1499059597315342829 ) ) ;
#8402 = PLANE ( 'NONE',  #6387 ) ;
#8403 = EDGE_CURVE ( 'NONE', #4881, #4325, #709, .T. ) ;
#8404 = PRODUCT_DEFINITION_SHAPE ( 'NONE', 'NONE',  #14624 ) ;
#8405 = CARTESIAN_POINT ( 'NONE',  ( 451.3035746174796827, 294.6698471414878782, -210.0000000000000000 ) ) ;
#8406 = UNCERTAINTY_MEASURE_WITH_UNIT (LENGTH_MEASURE( 1.000000000000000082E-05 ), #1077, 'distance_accuracy_value', 'NONE');
#8407 = LINE ( 'NONE', #13886, #10075 ) ;
#8408 = ORIENTED_EDGE ( 'NONE', *, *, #403, .F. ) ;
#8409 = DIRECTION ( 'NONE',  ( -0.000000000000000000, -0.000000000000000000, 1.000000000000000000 ) ) ;
#8410 = CARTESIAN_POINT ( 'NONE',  ( 5.416666666666667851, -4.378239541354669306, -5.848636054922037530 ) ) ;
#8411 = DIRECTION ( 'NONE',  ( 0.000000000000000000, 0.000000000000000000, -1.000000000000000000 ) ) ;
#8412 = AXIS2_PLACEMENT_3D ( 'NONE', #5176, #4967, #6139 ) ;
#8413 = CARTESIAN_POINT ( 'NONE',  ( 635.0000000000000000, 160.0000000000000284, -190.0000000000000000 ) ) ;
#8414 = AXIS2_PLACEMENT_3D ( 'NONE', #6760, #6700, #12521 ) ;
#8415 = ORIENTED_EDGE ( 'NONE', *, *, #322, .T. ) ;
#8416 = ORIENTED_EDGE ( 'NONE', *, *, #7472, .F. ) ;
#8417 = DIRECTION ( 'NONE',  ( 0.000000000000000000, 0.000000000000000000, 1.000000000000000000 ) ) ;
#8418 = DIRECTION ( 'NONE',  ( 0.000000000000000000, 0.000000000000000000, 1.000000000000000000 ) ) ;
#8419 = CARTESIAN_POINT ( 'NONE',  ( 721.0120664571321640, 218.1493915422654482, 177.5999999999999659 ) ) ;
#8420 = EDGE_CURVE ( 'NONE', #7485, #1897, #10034, .T. ) ;
#8422 = ORIENTED_EDGE ( 'NONE', *, *, #1504, .T. ) ;
#8421 = AXIS2_PLACEMENT_3D ( 'NONE', #12955, #9499, #7130 ) ;
#8423 = AXIS2_PLACEMENT_3D ( 'NONE', #4174, #8602, #8672 ) ;
#8424 = DIRECTION ( 'NONE',  ( -0.000000000000000000, -0.000000000000000000, -1.000000000000000000 ) ) ;
#8425 = FACE_OUTER_BOUND ( 'NONE', #12052, .T. ) ;
#8426 = DIRECTION ( 'NONE',  ( -1.000000000000000000, -0.000000000000000000, -0.000000000000000000 ) ) ;
#8427 = DIRECTION ( 'NONE',  ( 1.000000000000000000, 0.000000000000000000, 0.000000000000000000 ) ) ;
#8428 = DIRECTION ( 'NONE',  ( -0.000000000000000000, -0.000000000000000000, 1.000000000000000000 ) ) ;
#8429 = CARTESIAN_POINT ( 'NONE',  ( -3.983107665916332252, 5.570601890521282407, -6.171481112545251335 ) ) ;
#8430 = ORIENTED_EDGE ( 'NONE', *, *, #1784, .T. ) ;
#8431 = CARTESIAN_POINT ( 'NONE',  ( -4.024497503033714452, 2.323544716729487813, -3.572167766733750582 ) ) ;
#8432 = ORIENTED_EDGE ( 'NONE', *, *, #5130, .T. ) ;
#8433 = ORIENTED_EDGE ( 'NONE', *, *, #311, .F. ) ;
#8434 = CARTESIAN_POINT ( 'NONE',  ( -4.000000000000000000, 1.941961291383472732, -0.3515519931180205448 ) ) ;
#8435 = CIRCLE ( 'NONE', #10326, 2.649999999999985700 ) ;
#8436 = CIRCLE ( 'NONE', #2065, 4.199999999999981526 ) ;
#8437 = EDGE_CURVE ( 'NONE', #3502, #1376, #4978, .T. ) ;
#8438 = DIRECTION ( 'NONE',  ( 0.000000000000000000, 0.000000000000000000, 1.000000000000000000 ) ) ;
#8439 = CARTESIAN_POINT ( 'NONE',  ( 610.0000000000000000, 175.0000000000000568, 190.0000000000000000 ) ) ;
#8440 = CARTESIAN_POINT ( 'NONE',  ( 5.200000000000002842, 3.061616997868383634E-16, -2.500000000000000444 ) ) ;
#8441 = ORIENTED_EDGE ( 'NONE', *, *, #5612, .T. ) ;
#8442 = EDGE_CURVE ( 'NONE', #5487, #1005, #6849, .T. ) ;
#8443 = CARTESIAN_POINT ( 'NONE',  ( -4.000000000000000000, 0.000000000000000000, 0.000000000000000000 ) ) ;
#8444 = DIRECTION ( 'NONE',  ( -3.340694023494469140E-16, 4.069768234201303760E-15, 1.000000000000000000 ) ) ;
#8445 = VECTOR ( 'NONE', #1158, 1000.000000000000000 ) ;
#8446 = EDGE_CURVE ( 'NONE', #8156, #6317, #12616, .T. ) ;
#8447 = CIRCLE ( 'NONE', #4926, 2.499999999999946709 ) ;
#8448 = CARTESIAN_POINT ( 'NONE',  ( 2.500000000000000000, 2.357898499370431722, -2.818925648462311528E-15 ) ) ;
#8449 = DIRECTION ( 'NONE',  ( 1.000000000000000000, 0.000000000000000000, 0.000000000000000000 ) ) ;
#8450 =( LENGTH_UNIT ( ) NAMED_UNIT ( * ) SI_UNIT ( .MILLI., .METRE. ) );
#8451 = ORIENTED_EDGE ( 'NONE', *, *, #6287, .F. ) ;
#8452 = EDGE_CURVE ( 'NONE', #14303, #10624, #9528, .T. ) ;
#8453 =( LENGTH_UNIT ( ) NAMED_UNIT ( * ) SI_UNIT ( .MILLI., .METRE. ) );
#8454 = CARTESIAN_POINT ( 'NONE',  ( 0.1481481481481481122, -4.797713218419819903, 0.000000000000000000 ) ) ;
#8455 = ITEM_DEFINED_TRANSFORMATION ( 'NONE', 'NONE', #2408,  #9440 ) ;
#8456 = B_SPLINE_CURVE_WITH_KNOTS ( 'NONE', 3,
 ( #2895, #353, #6271, #12701, #4889, #8271, #12922, #11812 ),
 .UNSPECIFIED., .F., .F.,
 ( 4, 2, 2, 4 ),
 ( 0.002921158011986708155, 0.003648658599403063578, 0.004376159186819419435, 0.005831160361652130281 ),
 .UNSPECIFIED. ) ;
#8457 = ORIENTED_EDGE ( 'NONE', *, *, #14251, .T. ) ;
#8458 = VECTOR ( 'NONE', #7375, 1000.000000000000227 ) ;
#8459 = CARTESIAN_POINT ( 'NONE',  ( 3.999999999999999112, 2.309401076758497595, -3.504271511727124366 ) ) ;
#8460 = VECTOR ( 'NONE', #8282, 1000.000000000000000 ) ;
#8461 = FACE_OUTER_BOUND ( 'NONE', #4833, .T. ) ;
#8462 = DIRECTION ( 'NONE',  ( -1.000000000000000000, 0.000000000000000000, 0.000000000000000000 ) ) ;
#8463 =( BOUNDED_SURFACE ( )  B_SPLINE_SURFACE ( 3, 2, ( 
 ( #10958, #6393, #13255 ),
 ( #3146, #7648, #13040 ),
 ( #13317, #8753, #3208 ),
 ( #832, #10894, #12131 ),
 ( #2015, #6530, #11910 ),
 ( #1801, #6311, #8600 ) ),
 .UNSPECIFIED., .F., .F., .T. ) 
 B_SPLINE_SURFACE_WITH_KNOTS ( ( 4, 2, 4 ),
 ( 3, 3 ),
 ( 0.02367865728600888550, 0.02663179453327094853, 0.02958493178053300809 ),
 ( 0.000000000000000000, 1.000000000000000000 ),
 .UNSPECIFIED. ) 
 GEOMETRIC_REPRESENTATION_ITEM ( )  RATIONAL_B_SPLINE_SURFACE ( (
 ( 1.000000000000000000, 0.8047781103519400236, 1.000000000000000000),
 ( 1.000000000000000000, 0.8123785825980049946, 1.000000000000000000),
 ( 1.000000000000000000, 0.8190671539288042480, 1.000000000000000000),
 ( 1.000000000000000000, 0.8192352255335092481, 1.000000000000000000),
 ( 1.000000000000000000, 0.8126129676835895932, 1.000000000000000000),
 ( 1.000000000000000000, 0.8047712537969730073, 1.000000000000000000) ) ) 
 REPRESENTATION_ITEM ( '' )  SURFACE ( )  );
#8464 = ORIENTED_EDGE ( 'NONE', *, *, #12216, .T. ) ;
#8465 = FACE_OUTER_BOUND ( 'NONE', #14306, .T. ) ;
#8467 = EDGE_CURVE ( 'NONE', #3014, #2565, #3549, .T. ) ;
#8466 = CIRCLE ( 'NONE', #7287, 2.700000000000000622 ) ;
#8468 = CARTESIAN_POINT ( 'NONE',  ( -3.349226789952655547, -2.685125164760744809, -0.2236248678334863682 ) ) ;
#8469 = CARTESIAN_POINT ( 'NONE',  ( 6.500000000000000888, 0.000000000000000000, 0.000000000000000000 ) ) ;
#8470 = DIRECTION ( 'NONE',  ( -0.000000000000000000, -0.000000000000000000, -1.000000000000000000 ) ) ;
#8471 = ORIENTED_EDGE ( 'NONE', *, *, #12706, .F. ) ;
#8472 = VECTOR ( 'NONE', #10869, 1000.000000000000000 ) ;
#8473 = AXIS2_PLACEMENT_3D ( 'NONE', #13086, #12935, #2743 ) ;
#8474 = CARTESIAN_POINT ( 'NONE',  ( -4.197477534772231955, 0.8522413273724368521, -3.505042416683225692 ) ) ;
#8475 = LINE ( 'NONE', #8250, #9845 ) ;
#8476 = ORIENTED_EDGE ( 'NONE', *, *, #14531, .F. ) ;
#8477 = ORIENTED_EDGE ( 'NONE', *, *, #1214, .T. ) ;
#8478 = VERTEX_POINT ( 'NONE', #1542 ) ;
#8479 = CARTESIAN_POINT ( 'NONE',  ( 636.7717819724297215, 155.3244477714206653, 211.0000000000000000 ) ) ;
#8480 = AXIS2_PLACEMENT_3D ( 'NONE', #1793, #10800, #7479 ) ;
#8481 = ADVANCED_FACE ( 'NONE', ( #10629 ), #1325, .F. ) ;
#8482 = CYLINDRICAL_SURFACE ( 'NONE', #3280, 2.649999999999985700 ) ;
#8484 = CONICAL_SURFACE ( 'NONE', #4245, 2.059999999999998721, 0.9599310885968738161 ) ;
#8483 = DIRECTION ( 'NONE',  ( 0.000000000000000000, 0.000000000000000000, 1.000000000000000000 ) ) ;
#8485 = EDGE_CURVE ( 'NONE', #3563, #2314, #8488, .T. ) ;
#8486 = CONICAL_SURFACE ( 'NONE', #6373, 2.041999999999999815, 1.047197551196591858 ) ;
#8487 = CARTESIAN_POINT ( 'NONE',  ( 1.500000000000001332, 0.000000000000000000, 0.000000000000000000 ) ) ;
#8488 = B_SPLINE_CURVE_WITH_KNOTS ( 'NONE', 3,
 ( #3629, #8046, #11646, #1396 ),
 .UNSPECIFIED., .F., .F.,
 ( 4, 4 ),
 ( 0.000000000000000000, 0.002452478801916361129 ),
 .UNSPECIFIED. ) ;
#8489 = VECTOR ( 'NONE', #4155, 1000.000000000000227 ) ;
#8490 = LINE ( 'NONE', #8338, #8619 ) ;
#8491 = ORIENTED_EDGE ( 'NONE', *, *, #9527, .T. ) ;
#8492 = AXIS2_PLACEMENT_3D ( 'NONE', #9541, #10645, #5991 ) ;
#8493 = CARTESIAN_POINT ( 'NONE',  ( 2.500000000000000000, 0.000000000000000000, 0.000000000000000000 ) ) ;
#8494 = CARTESIAN_POINT ( 'NONE',  ( 721.0120664571322777, 218.1493915422639702, -177.6000000000007617 ) ) ;
#8495 = DIRECTION ( 'NONE',  ( 0.000000000000000000, 0.000000000000000000, 1.000000000000000000 ) ) ;
#8496 = VECTOR ( 'NONE', #10589, 1000.000000000000114 ) ;
#8497 = PLANE ( 'NONE',  #13693 ) ;
#8498 = VECTOR ( 'NONE', #3937, 1000.000000000000000 ) ;
#8499 = ORIENTED_EDGE ( 'NONE', *, *, #523, .T. ) ;
#8500 = ORIENTED_EDGE ( 'NONE', *, *, #11359, .T. ) ;
#8501 = CARTESIAN_POINT ( 'NONE',  ( 635.0000000000000000, 160.0000000000000284, -225.5000000000000000 ) ) ;
#8502 = DIRECTION ( 'NONE',  ( -0.9578262852211513190, 0.2873478855663453846, 0.000000000000000000 ) ) ;
#8503 = CARTESIAN_POINT ( 'NONE',  ( 609.8294541519869654, 189.4056243435263980, -189.7329333695814739 ) ) ;
#8504 = AXIS2_PLACEMENT_3D ( 'NONE', #9369, #9450, #13956 ) ;
#8505 = FACE_OUTER_BOUND ( 'NONE', #1905, .T. ) ;
#8506 = AXIS2_PLACEMENT_3D ( 'NONE', #1531, #1313, #1246 ) ;
#8507 = ORIENTED_EDGE ( 'NONE', *, *, #8993, .F. ) ;
#8508 =( GEOMETRIC_REPRESENTATION_CONTEXT ( 3 ) GLOBAL_UNCERTAINTY_ASSIGNED_CONTEXT ( ( #6498 ) ) GLOBAL_UNIT_ASSIGNED_CONTEXT ( ( #6489, #3167, #2943 ) ) REPRESENTATION_CONTEXT ( 'NONE', 'WORKASPACE' ) );
#8509 = CARTESIAN_POINT ( 'NONE',  ( -8.505790995054899994, 376.6597771564184427, 184.8000000000000398 ) ) ;
#8510 = CARTESIAN_POINT ( 'NONE',  ( -0.2259792476677698891, 7.636022678937394836, -6.470294263593361350 ) ) ;
#8511 = DIRECTION ( 'NONE',  ( -1.000000000000000000, 0.000000000000000000, 0.000000000000000000 ) ) ;
#8512 = DIRECTION ( 'NONE',  ( -1.000000000000000000, 0.000000000000000000, 0.000000000000000000 ) ) ;
#8513 = DIRECTION ( 'NONE',  ( -0.9237280213470676626, -0.3830490080632388272, 0.000000000000000000 ) ) ;
#8514 = CARTESIAN_POINT ( 'NONE',  ( 142.4540310085880606, 355.9707293956415697, -190.0000000000000000 ) ) ;
#8515 = CIRCLE ( 'NONE', #10402, 4.199999999999926459 ) ;
#8516 = EDGE_CURVE ( 'NONE', #12301, #6413, #10544, .T. ) ;
#8517 = ORIENTED_EDGE ( 'NONE', *, *, #8696, .T. ) ;
#8518 = CIRCLE ( 'NONE', #7562, 5.000000000000004441 ) ;
#8519 = DIRECTION ( 'NONE',  ( 1.000000000000000000, 0.000000000000000000, 0.000000000000000000 ) ) ;
#8520 = EDGE_LOOP ( 'NONE', ( #7548, #8329, #13332, #13684 ) ) ;
#8521 = ORIENTED_EDGE ( 'NONE', *, *, #3377, .T. ) ;
#8522 = CARTESIAN_POINT ( 'NONE',  ( -9.999999999999998224, 376.8992337277234128, 187.0000000000000000 ) ) ;
#8523 = AXIS2_PLACEMENT_3D ( 'NONE', #5235, #495, #13117 ) ;
#8524 =( GEOMETRIC_REPRESENTATION_CONTEXT ( 3 ) GLOBAL_UNCERTAINTY_ASSIGNED_CONTEXT ( ( #12696 ) ) GLOBAL_UNIT_ASSIGNED_CONTEXT ( ( #9936, #1962, #10820 ) ) REPRESENTATION_CONTEXT ( 'NONE', 'WORKASPACE' ) );
#8525 = LINE ( 'NONE', #10809, #3790 ) ;
#8526 = AXIS2_PLACEMENT_3D ( 'NONE', #2250, #8087, #4708 ) ;
#8527 = DIRECTION ( 'NONE',  ( 0.000000000000000000, 0.000000000000000000, -1.000000000000000000 ) ) ;
#8528 = CARTESIAN_POINT ( 'NONE',  ( 635.0000000000000000, 160.0000000000000284, -210.0000119999999981 ) ) ;
#8529 = ORIENTED_EDGE ( 'NONE', *, *, #6481, .T. ) ;
#8530 = LINE ( 'NONE', #13106, #5889 ) ;
#8531 = CARTESIAN_POINT ( 'NONE',  ( 611.4942090049448780, 232.4210031920607378, -190.0000000000000000 ) ) ;
#8532 = EDGE_CURVE ( 'NONE', #2671, #12527, #9231, .T. ) ;
#8533 = EDGE_LOOP ( 'NONE', ( #2809, #12857, #2204, #1157 ) ) ;
#8534 = CARTESIAN_POINT ( 'NONE',  ( 446.3084422793565409, 264.0194060144110608, -187.0000000000000000 ) ) ;
#8535 = CARTESIAN_POINT ( 'NONE',  ( 629.0000000000000000, 154.0000000000000284, -187.5000000000000000 ) ) ;
#8536 = CONTEXT_DEPENDENT_SHAPE_REPRESENTATION ( #747, #8541 ) ;
#8537 = ORIENTED_EDGE ( 'NONE', *, *, #13714, .F. ) ;
#8538 = AXIS2_PLACEMENT_3D ( 'NONE', #10026, #14532, #7826 ) ;
#8539 = EDGE_CURVE ( 'NONE', #2766, #4352, #9695, .T. ) ;
#8540 = FACE_BOUND ( 'NONE', #1768, .T. ) ;
#8541 = PRODUCT_DEFINITION_SHAPE ( 'NONE', 'NONE',  #14633 ) ;
#8542 = EDGE_CURVE ( 'NONE', #10517, #10228, #5218, .T. ) ;
#8543 = AXIS2_PLACEMENT_3D ( 'NONE', #13004, #5107, #12924 ) ;
#8544 = CARTESIAN_POINT ( 'NONE',  ( -6.500000000000006217, 3.752776749732561257, -6.177802698399960768 ) ) ;
#8545 = PLANE ( 'NONE',  #2145 ) ;
#8546 = ADVANCED_FACE ( 'NONE', ( #3770 ), #9686, .F. ) ;
#8547 = AXIS2_PLACEMENT_3D ( 'NONE', #8692, #7509, #9952 ) ;
#8548 = ORIENTED_EDGE ( 'NONE', *, *, #10596, .F. ) ;
#8549 = DIRECTION ( 'NONE',  ( -1.000000000000000000, -0.000000000000000000, -0.000000000000000000 ) ) ;
#8550 = CARTESIAN_POINT ( 'NONE',  ( -4.000000000000000000, -2.309401076758512694, -5.000000000000000000 ) ) ;
#8551 = LINE ( 'NONE', #2942, #13264 ) ;
#8552 = DIRECTION ( 'NONE',  ( 0.000000000000000000, 0.000000000000000000, 1.000000000000000000 ) ) ;
#8553 = VERTEX_POINT ( 'NONE', #11500 ) ;
#8554 = PRODUCT ( 'angular contact ball bearing_68_iso_ISO 15 ABB - 1710 - 20,SI,NC,20_68', 'angular contact ball bearing_68_iso_ISO 15 ABB - 1710 - 20,SI,NC,20_68', '', ( #4513 ) ) ;
#8555 = CARTESIAN_POINT ( 'NONE',  ( 1.600000000000000089, 0.000000000000000000, 0.000000000000000000 ) ) ;
#8556 = PRESENTATION_STYLE_ASSIGNMENT (( #9446 ) ) ;
#8557 = CARTESIAN_POINT ( 'NONE',  ( -6.499999999999999112, 1.286902272306389428, -0.09436334093186068972 ) ) ;
#8558 = EDGE_LOOP ( 'NONE', ( #10193, #11770, #2522, #4591 ) ) ;
#8559 = ORIENTED_EDGE ( 'NONE', *, *, #9279, .T. ) ;
#8560 = CIRCLE ( 'NONE', #10213, 5.000000000000004441 ) ;
#8561 = CARTESIAN_POINT ( 'NONE',  ( -8.505790995054940851, 376.6597771564182722, 190.0000000000000284 ) ) ;
#8562 = EDGE_CURVE ( 'NONE', #13362, #1078, #961, .T. ) ;
#8563 = EDGE_CURVE ( 'NONE', #604, #14470, #2850, .T. ) ;
#8564 = CARTESIAN_POINT ( 'NONE',  ( 3.309651814758564736, -5.455921364805393026, -1.000000000000000000 ) ) ;
#8565 = CARTESIAN_POINT ( 'NONE',  ( 6.323279575526313145, 3.325091652215454108, -4.240772318536886409 ) ) ;
#8566 = ADVANCED_FACE ( 'NONE', ( #3849 ), #8330, .T. ) ;
#8567 = B_SPLINE_CURVE_WITH_KNOTS ( 'NONE', 3,
 ( #2391, #2302, #9330, #3656, #11535, #6818, #303, #8136, #4547, #1209, #10220, #12642, #9181, #2530, #7033, #4837 ),
 .UNSPECIFIED., .F., .F.,
 ( 4, 3, 3, 3, 3, 4 ),
 ( 0.000000000000000000, 5.303647860849277479E-05, 0.0001057093501027509761, 0.0001642058037233847250, 0.0002210073443967694375, 0.0002236769549551750945 ),
 .UNSPECIFIED. ) ;
#8568 = DIRECTION ( 'NONE',  ( -1.000000000000000000, -0.000000000000000000, -0.000000000000000000 ) ) ;
#8569 = FACE_OUTER_BOUND ( 'NONE', #1610, .T. ) ;
#8570 = ORIENTED_EDGE ( 'NONE', *, *, #13921, .F. ) ;
#8571 = FACE_OUTER_BOUND ( 'NONE', #7846, .T. ) ;
#8572 = DIRECTION ( 'NONE',  ( 0.000000000000000000, 0.000000000000000000, 1.000000000000000000 ) ) ;
#8573 = PRODUCT_CONTEXT ( 'NONE', #1022, 'mechanical' ) ;
#8574 = DIRECTION ( 'NONE',  ( -0.2873478855663454401, -0.9578262852211514300, 0.000000000000000000 ) ) ;
#8575 = VERTEX_POINT ( 'NONE', #6125 ) ;
#8576 = ORIENTED_EDGE ( 'NONE', *, *, #12240, .F. ) ;
#8577 = DIRECTION ( 'NONE',  ( 1.224646799147353207E-16, 1.000000000000000000, 0.000000000000000000 ) ) ;
#8578 = DIRECTION ( 'NONE',  ( -0.000000000000000000, -0.000000000000000000, 1.000000000000000000 ) ) ;
#8579 = CARTESIAN_POINT ( 'NONE',  ( 6.323279575526388641, 5.335162385629701909, 0.7592276814629709270 ) ) ;
#8580 =( REPRESENTATION_RELATIONSHIP ('NONE','NONE', #2822, #2248 ) REPRESENTATION_RELATIONSHIP_WITH_TRANSFORMATION ( #3329 )SHAPE_REPRESENTATION_RELATIONSHIP( ) );
#8581 = CARTESIAN_POINT ( 'NONE',  ( 0.1481481481481481122, -4.797713218419819903, -1.000000000000000000 ) ) ;
#8582 = ORIENTED_EDGE ( 'NONE', *, *, #9878, .T. ) ;
#8583 = PLANE ( 'NONE',  #1008 ) ;
#8584 = LINE ( 'NONE', #10726, #11595 ) ;
#8585 = CARTESIAN_POINT ( 'NONE',  ( 0.000000000000000000, -3.464101615137750834, 2.000000000000007994 ) ) ;
#8586 = EDGE_LOOP ( 'NONE', ( #11824, #5309 ) ) ;
#8587 = LINE ( 'NONE', #6158, #14103 ) ;
#8588 = CARTESIAN_POINT ( 'NONE',  ( -2.832728918602883006, -6.234773369952733901, -6.171481112545254000 ) ) ;
#8589 = LINE ( 'NONE', #4162, #1133 ) ;
#8590 = ORIENTED_EDGE ( 'NONE', *, *, #6048, .F. ) ;
#8591 = CARTESIAN_POINT ( 'NONE',  ( 635.0000000000000000, 235.0000000000000284, -263.5000000000000000 ) ) ;
#8592 = ORIENTED_EDGE ( 'NONE', *, *, #10915, .T. ) ;
#8593 = ORIENTED_EDGE ( 'NONE', *, *, #1526, .F. ) ;
#8594 = DIRECTION ( 'NONE',  ( 1.000000000000000000, 0.000000000000000000, 0.000000000000000000 ) ) ;
#8595 = CARTESIAN_POINT ( 'NONE',  ( -10.00000000000000000, -10.00000000000000000, 210.0000000000000000 ) ) ;
#8596 = EDGE_CURVE ( 'NONE', #4352, #10367, #2129, .T. ) ;
#8597 = ORIENTED_EDGE ( 'NONE', *, *, #12372, .T. ) ;
#8598 = ADVANCED_FACE ( 'NONE', ( #781 ), #6691, .F. ) ;
#8599 = ORIENTED_EDGE ( 'NONE', *, *, #7319, .T. ) ;
#8600 = CARTESIAN_POINT ( 'NONE',  ( 6.541334219041336162, -2.934241909852036034, 5.143243597038031467 ) ) ;
#8601 = CARTESIAN_POINT ( 'NONE',  ( 6.832273232158034837, 3.329759989367264694, -6.449140625371624580 ) ) ;
#8602 = DIRECTION ( 'NONE',  ( 9.304756960132325412E-16, 6.965275210156238168E-15, 1.000000000000000000 ) ) ;
#8603 = DIRECTION ( 'NONE',  ( -1.000000000000000000, -0.000000000000000000, -0.000000000000000000 ) ) ;
#8604 =( NAMED_UNIT ( * ) PLANE_ANGLE_UNIT ( ) SI_UNIT ( $, .RADIAN. ) );
#8605 = VERTEX_POINT ( 'NONE', #4335 ) ;
#8606 = CARTESIAN_POINT ( 'NONE',  ( 609.7206935199311602, 188.0285076711449790, 189.0295014234984023 ) ) ;
#8607 = CARTESIAN_POINT ( 'NONE',  ( 1.400000000000001910, 0.000000000000000000, 0.000000000000000000 ) ) ;
#8608 = ORIENTED_EDGE ( 'NONE', *, *, #11746, .F. ) ;
#8609 = DIRECTION ( 'NONE',  ( 0.2873478855663453846, 0.9578262852211513190, 0.000000000000000000 ) ) ;
#8610 = ORIENTED_EDGE ( 'NONE', *, *, #4321, .T. ) ;
#8611 = DIRECTION ( 'NONE',  ( -1.000000000000000000, 3.784851220313450466E-14, 0.000000000000000000 ) ) ;
#8612 = EDGE_CURVE ( 'NONE', #358, #11016, #8832, .T. ) ;
#8613 = FACE_OUTER_BOUND ( 'NONE', #11730, .T. ) ;
#8614 = ORIENTED_EDGE ( 'NONE', *, *, #2130, .T. ) ;
#8615 = CARTESIAN_POINT ( 'NONE',  ( 2.000000000000005329, -3.464101615137751722, 0.000000000000000000 ) ) ;
#8616 = DIRECTION ( 'NONE',  ( -1.000000000000000000, 0.000000000000000000, 0.000000000000000000 ) ) ;
#8617 = CARTESIAN_POINT ( 'NONE',  ( 2.000000000000000000, -6.429618962271402616, -1.000000000000000000 ) ) ;
#8618 = SURFACE_STYLE_FILL_AREA ( #10837 ) ;
#8619 = VECTOR ( 'NONE', #8186, 1000.000000000000000 ) ;
#8620 = ORIENTED_EDGE ( 'NONE', *, *, #8848, .T. ) ;
#8621 = EDGE_CURVE ( 'NONE', #3017, #9599, #915, .T. ) ;
#8622 = CARTESIAN_POINT ( 'NONE',  ( -10.00000000000004263, 371.6790804732683569, -169.9999999999999716 ) ) ;
#8623 = CARTESIAN_POINT ( 'NONE',  ( -6.500000000000000000, 1.602771114417265164, -0.1495523863686162858 ) ) ;
#8624 = ORIENTED_EDGE ( 'NONE', *, *, #12878, .T. ) ;
#8625 = ADVANCED_BREP_SHAPE_REPRESENTATION ( '', ( #2587, #9440 ), #8524 ) ;
#8626 = ORIENTED_EDGE ( 'NONE', *, *, #8174, .F. ) ;
#8627 = CARTESIAN_POINT ( 'NONE',  ( 6.837824896291514243, -3.947820044545437224, -6.564402953523717166 ) ) ;
#8628 = CARTESIAN_POINT ( 'NONE',  ( 0.000000000000000000, 0.000000000000000000, 190.0000000000000000 ) ) ;
#8629 = EDGE_CURVE ( 'NONE', #5999, #2671, #4260, .T. ) ;
#8630 = CARTESIAN_POINT ( 'NONE',  ( 6.092449800118089343, 3.827241605637790034, -3.371023086193853047 ) ) ;
#8631 = DIRECTION ( 'NONE',  ( 0.000000000000000000, 0.000000000000000000, -1.000000000000000000 ) ) ;
#8632 = LINE ( 'NONE', #12022, #8647 ) ;
#8633 = EDGE_CURVE ( 'NONE', #4325, #1059, #11095, .T. ) ;
#8634 = ORIENTED_EDGE ( 'NONE', *, *, #11155, .F. ) ;
#8635 = EDGE_CURVE ( 'NONE', #8873, #10698, #13397, .T. ) ;
#8636 = DIRECTION ( 'NONE',  ( -0.9578262852211515410, 0.2873478855663446074, 0.000000000000000000 ) ) ;
#8637 = CARTESIAN_POINT ( 'NONE',  ( 0.1586754815284860953, 2.687817229851475531, -3.344563996438206566 ) ) ;
#8638 = DIRECTION ( 'NONE',  ( 1.000000000000000000, 0.000000000000000000, 0.000000000000000000 ) ) ;
#8640 = EDGE_CURVE ( 'NONE', #5994, #5405, #12141, .T. ) ;
#8639 = CARTESIAN_POINT ( 'NONE',  ( 451.6722694765949768, 316.6998517015743460, 210.0000000000000000 ) ) ;
#8641 = ORIENTED_EDGE ( 'NONE', *, *, #8240, .T. ) ;
#8642 = PRODUCT_DEFINITION ( 'UNKNOWN', '', #5255, #7232 ) ;
#8643 = ORIENTED_EDGE ( 'NONE', *, *, #2670, .F. ) ;
#8644 = DIRECTION ( 'NONE',  ( 0.8660254037844374864, -0.5000000000000018874, 0.000000000000000000 ) ) ;
#8645 = LINE ( 'NONE', #13149, #8725 ) ;
#8646 = CARTESIAN_POINT ( 'NONE',  ( 609.6939753585367043, 187.4861613156657540, -188.5968284039610978 ) ) ;
#8647 = VECTOR ( 'NONE', #12098, 1000.000000000000114 ) ;
#8648 = DIRECTION ( 'NONE',  ( 0.000000000000000000, 0.000000000000000000, -1.000000000000000000 ) ) ;
#8649 = ORIENTED_EDGE ( 'NONE', *, *, #4200, .T. ) ;
#8650 = CARTESIAN_POINT ( 'NONE',  ( -6.500000000000000888, 4.012863338656273982, -6.470131626772281486 ) ) ;
#8651 = EDGE_LOOP ( 'NONE', ( #12169, #6936, #12926, #6828, #8158 ) ) ;
#8652 = VECTOR ( 'NONE', #1841, 1000.000000000000000 ) ;
#8653 = VECTOR ( 'NONE', #1301, 1000.000000000000000 ) ;
#8654 = CARTESIAN_POINT ( 'NONE',  ( 629.0000000000000000, 154.0000000000000284, -187.5000000000000000 ) ) ;
#8655 = CARTESIAN_POINT ( 'NONE',  ( -9.999999999999957367, 376.8992337277236970, 187.0000000000000000 ) ) ;
#8656 = DIRECTION ( 'NONE',  ( -0.000000000000000000, -0.000000000000000000, 1.000000000000000000 ) ) ;
#8657 =( NAMED_UNIT ( * ) SI_UNIT ( $, .STERADIAN. ) SOLID_ANGLE_UNIT ( ) );
#8658 = PRODUCT_DEFINITION_SHAPE ( 'NONE', 'NONE',  #14515 ) ;
#8659 = ORIENTED_EDGE ( 'NONE', *, *, #9883, .F. ) ;
#8660 = DIRECTION ( 'NONE',  ( -1.000000000000000000, -0.000000000000000000, -0.000000000000000000 ) ) ;
#8661 = EDGE_LOOP ( 'NONE', ( #8236, #8348 ) ) ;
#8662 = ORIENTED_EDGE ( 'NONE', *, *, #8596, .F. ) ;
#8663 = DIRECTION ( 'NONE',  ( 0.000000000000000000, 0.000000000000000000, -1.000000000000000000 ) ) ;
#8664 = ADVANCED_FACE ( 'NONE', ( #5573 ), #11034, .T. ) ;
#8665 = DIRECTION ( 'NONE',  ( -0.000000000000000000, -0.000000000000000000, -1.000000000000000000 ) ) ;
#8666 = VECTOR ( 'NONE', #5940, 1000.000000000000114 ) ;
#8667 = ADVANCED_FACE ( 'NONE', ( #14448 ), #14174, .T. ) ;
#8668 = ORIENTED_EDGE ( 'NONE', *, *, #11070, .F. ) ;
#8669 = VERTEX_POINT ( 'NONE', #2025 ) ;
#8670 = DIRECTION ( 'NONE',  ( -1.000000000000000000, 0.000000000000000000, 0.000000000000000000 ) ) ;
#8671 = CARTESIAN_POINT ( 'NONE',  ( 6.500000000000000888, 1.333904739168207065, -6.094327662196326933 ) ) ;
#8672 = DIRECTION ( 'NONE',  ( 0.000000000000000000, -1.000000000000000000, 6.965275210156238168E-15 ) ) ;
#8673 = CYLINDRICAL_SURFACE ( 'NONE', #13280, 0.7500000000000000000 ) ;
#8674 = VERTEX_POINT ( 'NONE', #14293 ) ;
#8675 = MECHANICAL_DESIGN_GEOMETRIC_PRESENTATION_REPRESENTATION (  '', ( #8188 ), #13858 ) ;
#8676 =( LENGTH_UNIT ( ) NAMED_UNIT ( * ) SI_UNIT ( .MILLI., .METRE. ) );
#8677 = PLANE ( 'NONE',  #8926 ) ;
#8678 = CONTEXT_DEPENDENT_SHAPE_REPRESENTATION ( #7258, #159 ) ;
#8679 = VECTOR ( 'NONE', #7696, 1000.000000000000000 ) ;
#8680 = VERTEX_POINT ( 'NONE', #1969 ) ;
#8681 = DIRECTION ( 'NONE',  ( 1.000000000000000000, 0.000000000000000000, 0.000000000000000000 ) ) ;
#8682 = ADVANCED_FACE ( 'NONE', ( #3290 ), #4181, .F. ) ;
#8683 = ORIENTED_EDGE ( 'NONE', *, *, #10805, .F. ) ;
#8684 = DIRECTION ( 'NONE',  ( 0.000000000000000000, 0.000000000000000000, -1.000000000000000000 ) ) ;
#8685 = LINE ( 'NONE', #5020, #14413 ) ;
#8686 = CIRCLE ( 'NONE', #6095, 7.500000000000000000 ) ;
#8687 =( GEOMETRIC_REPRESENTATION_CONTEXT ( 3 ) GLOBAL_UNCERTAINTY_ASSIGNED_CONTEXT ( ( #12557 ) ) GLOBAL_UNIT_ASSIGNED_CONTEXT ( ( #8212, #10580, #1650 ) ) REPRESENTATION_CONTEXT ( 'NONE', 'WORKASPACE' ) );
#8688 = AXIS2_PLACEMENT_3D ( 'NONE', #4444, #9773, #10422 ) ;
#8689 = EDGE_LOOP ( 'NONE', ( #8306, #8385, #2039, #4613, #7262, #10315 ) ) ;
#8690 = DIRECTION ( 'NONE',  ( 1.000000000000000000, 0.000000000000000000, 0.000000000000000000 ) ) ;
#8691 = LINE ( 'NONE', #8550, #7058 ) ;
#8692 = CARTESIAN_POINT ( 'NONE',  ( 0.000000000000000000, 7.654042494670957606E-16, -6.250000000000000000 ) ) ;
#8693 = VERTEX_POINT ( 'NONE', #2096 ) ;
#8694 = DIRECTION ( 'NONE',  ( -0.000000000000000000, -0.000000000000000000, 1.000000000000000000 ) ) ;
#8695 = EDGE_LOOP ( 'NONE', ( #9762, #3750, #4797, #5325, #409, #4994 ) ) ;
#8696 = EDGE_CURVE ( 'NONE', #4375, #12665, #11117, .T. ) ;
#8697 = AXIS2_PLACEMENT_3D ( 'NONE', #490, #12125, #10749 ) ;
#8698 = CIRCLE ( 'NONE', #13415, 2.199999999999757705 ) ;
#8699 = ORIENTED_EDGE ( 'NONE', *, *, #13451, .F. ) ;
#8700 = DIRECTION ( 'NONE',  ( -0.9237280213470682178, -0.3830490080632377725, 0.000000000000000000 ) ) ;
#8701 = DIRECTION ( 'NONE',  ( 9.794481010665704304E-16, 3.264827003555234768E-15, -1.000000000000000000 ) ) ;
#8702 =( GEOMETRIC_REPRESENTATION_CONTEXT ( 3 ) GLOBAL_UNCERTAINTY_ASSIGNED_CONTEXT ( ( #3260 ) ) GLOBAL_UNIT_ASSIGNED_CONTEXT ( ( #9668, #14171, #14459 ) ) REPRESENTATION_CONTEXT ( 'NONE', 'WORKASPACE' ) );
#8703 = CARTESIAN_POINT ( 'NONE',  ( 0.000000000000000000, 0.000000000000000000, 0.000000000000000000 ) ) ;
#8704 = CARTESIAN_POINT ( 'NONE',  ( 636.7009106935324780, 155.5114698605638637, 211.0000000000000000 ) ) ;
#8705 = AXIS2_PLACEMENT_3D ( 'NONE', #7843, #9261, #2061 ) ;
#8706 = AXIS2_PLACEMENT_3D ( 'NONE', #11262, #11411, #1300 ) ;
#8707 = B_SPLINE_CURVE_WITH_KNOTS ( 'NONE', 3,
 ( #4216, #13218, #7614, #1992, #6503, #10991, #9007, #4364 ),
 .UNSPECIFIED., .F., .F.,
 ( 4, 2, 2, 4 ),
 ( 8.442967473282902092E-20, 0.001493104274552340370, 0.002986208549104680740, 0.005972417098209361480 ),
 .UNSPECIFIED. ) ;
#8708 = PRODUCT_DEFINITION_CONTEXT ( 'detailed design', #7349, 'design' ) ;
#8709 = DIRECTION ( 'NONE',  ( 0.000000000000000000, 0.000000000000000000, 1.000000000000000000 ) ) ;
#8710 = ORIENTED_EDGE ( 'NONE', *, *, #10516, .T. ) ;
#8711 = LINE ( 'NONE', #8856, #9155 ) ;
#8712 = CARTESIAN_POINT ( 'NONE',  ( 3.250000000000003109, -5.629165124598849879, 0.000000000000000000 ) ) ;
#8713 = ADVANCED_FACE ( 'NONE', ( #10008 ), #5514, .T. ) ;
#8714 = AXIS2_PLACEMENT_3D ( 'NONE', #254, #2479, #6981 ) ;
#8715 = DIRECTION ( 'NONE',  ( -0.9578262852211513190, 0.2873478855663453846, 0.000000000000000000 ) ) ;
#8716 = ORIENTED_EDGE ( 'NONE', *, *, #1425, .F. ) ;
#8717 = ORIENTED_EDGE ( 'NONE', *, *, #13527, .T. ) ;
#8718 = DIRECTION ( 'NONE',  ( 0.000000000000000000, 0.000000000000000000, -1.000000000000000000 ) ) ;
#8719 = LINE ( 'NONE', #6510, #708 ) ;
#8720 = ADVANCED_FACE ( 'NONE', ( #2180 ), #8264, .T. ) ;
#8721 = CIRCLE ( 'NONE', #7057, 2.500000000000000444 ) ;
#8722 = VECTOR ( 'NONE', #14008, 1000.000000000000000 ) ;
#8723 = CARTESIAN_POINT ( 'NONE',  ( -5.416666666666667851, -4.378239541354669306, -5.848636054922036642 ) ) ;
#8724 = ADVANCED_FACE ( 'NONE', ( #10906 ), #10967, .F. ) ;
#8725 = VECTOR ( 'NONE', #1931, 1000.000000000000000 ) ;
#8726 = LINE ( 'NONE', #8939, #12021 ) ;
#8727 = VECTOR ( 'NONE', #2223, 1000.000000000000000 ) ;
#8728 = VERTEX_POINT ( 'NONE', #6406 ) ;
#8729 = ADVANCED_FACE ( 'NONE', ( #841 ), #7935, .F. ) ;
#8730 = CARTESIAN_POINT ( 'NONE',  ( -6.815701034932152069, -1.328907527188669668, -6.169383458210047522 ) ) ;
#8731 = ORIENTED_EDGE ( 'NONE', *, *, #4385, .T. ) ;
#8732 = AXIS2_PLACEMENT_3D ( 'NONE', #10971, #8977, #5362 ) ;
#8733 = CIRCLE ( 'NONE', #14167, 2.500000000000000444 ) ;
#8734 = CARTESIAN_POINT ( 'NONE',  ( 0.000000000000000000, 0.000000000000000000, 0.000000000000000000 ) ) ;
#8735 = CARTESIAN_POINT ( 'NONE',  ( 642.0000000000000000, 153.0000000000000284, -225.5000000000000000 ) ) ;
#8736 = FACE_OUTER_BOUND ( 'NONE', #12215, .T. ) ;
#8737 = VERTEX_POINT ( 'NONE', #9047 ) ;
#8738 = DIRECTION ( 'NONE',  ( 0.000000000000000000, 0.000000000000000000, 1.000000000000000000 ) ) ;
#8739 = ORIENTED_EDGE ( 'NONE', *, *, #14145, .F. ) ;
#8740 = ORIENTED_EDGE ( 'NONE', *, *, #3135, .T. ) ;
#8741 = CIRCLE ( 'NONE', #13938, 2.054999999999999716 ) ;
#8742 = DIRECTION ( 'NONE',  ( -0.2873478855663453846, -0.9578262852211513190, -0.000000000000000000 ) ) ;
#8743 = CIRCLE ( 'NONE', #2116, 5.249999999999976907 ) ;
#8744 = EDGE_CURVE ( 'NONE', #13147, #5903, #10152, .T. ) ;
#8745 = EDGE_CURVE ( 'NONE', #2446, #9530, #2469, .T. ) ;
#8746 = CARTESIAN_POINT ( 'NONE',  ( -3.680118525130244400, 2.494084732383327285, -0.3507732604232449702 ) ) ;
#8747 = B_SPLINE_CURVE_WITH_KNOTS ( 'NONE', 3,
 ( #11194, #13625, #4567, #5662 ),
 .UNSPECIFIED., .F., .F.,
 ( 4, 4 ),
 ( 0.000000000000000000, 0.002452478801916376308 ),
 .UNSPECIFIED. ) ;
#8748 = B_SPLINE_CURVE_WITH_KNOTS ( 'NONE', 3,
 ( #14612, #11827, #4730, #5679, #13567, #107 ),
 .UNSPECIFIED., .F., .F.,
 ( 4, 2, 4 ),
 ( 0.002336974151641552089, 0.003500975885716441950, 0.004664977619791332679 ),
 .UNSPECIFIED. ) ;
#8749 = ORIENTED_EDGE ( 'NONE', *, *, #1326, .F. ) ;
#8750 = ADVANCED_FACE ( 'NONE', ( #4555, #4700, #13549 ), #13770, .F. ) ;
#8751 = AXIS2_PLACEMENT_3D ( 'NONE', #5985, #2804, #11655 ) ;
#8752 = VERTEX_POINT ( 'NONE', #6826 ) ;
#8753 = CARTESIAN_POINT ( 'NONE',  ( 6.207530437345012864, -4.849805425594809094, 1.599890596046773972 ) ) ;
#8754 = CARTESIAN_POINT ( 'NONE',  ( 6.500000000000301981, 0.6542365398607151716, -6.055391205186719361 ) ) ;
#8755 = VECTOR ( 'NONE', #3373, 1000.000000000000000 ) ;
#8756 = FACE_OUTER_BOUND ( 'NONE', #3258, .T. ) ;
#8757 = FACE_OUTER_BOUND ( 'NONE', #7193, .T. ) ;
#8758 = FACE_OUTER_BOUND ( 'NONE', #321, .T. ) ;
#8759 = SHAPE_REPRESENTATION_RELATIONSHIP ( 'NONE' , 'NONE' ,  #748, #3692 ) ;
#8760 = ORIENTED_EDGE ( 'NONE', *, *, #3226, .F. ) ;
#8761 = VECTOR ( 'NONE', #8980, 1000.000000000000000 ) ;
#8762 = COLOUR_RGB ( '',0.8941176470588234615, 0.8941176470588234615, 0.8941176470588234615 ) ;
#8763 = PLANE ( 'NONE',  #13900 ) ;
#8764 = CONTEXT_DEPENDENT_SHAPE_REPRESENTATION ( #8199, #864 ) ;
#8765 = ORIENTED_EDGE ( 'NONE', *, *, #7774, .T. ) ;
#8766 = CARTESIAN_POINT ( 'NONE',  ( 3.500000000000000000, 0.000000000000000000, 0.000000000000000000 ) ) ;
#8767 = ORIENTED_EDGE ( 'NONE', *, *, #6873, .T. ) ;
#8768 = AXIS2_PLACEMENT_3D ( 'NONE', #5970, #6255, #3909 ) ;
#8769 = DIRECTION ( 'NONE',  ( -1.000000000000000000, 0.000000000000000000, 0.000000000000000000 ) ) ;
#8770 = CARTESIAN_POINT ( 'NONE',  ( 145.1678582058265476, 408.6511750828048548, -190.0000000000000000 ) ) ;
#8771 = STYLED_ITEM ( 'NONE', ( #4314 ), #13030 ) ;
#8772 = ORIENTED_EDGE ( 'NONE', *, *, #7350, .F. ) ;
#8773 = CARTESIAN_POINT ( 'NONE',  ( 610.6379424248335681, 188.7103817868187150, 185.3679143846944157 ) ) ;
#8774 = DIRECTION ( 'NONE',  ( 0.000000000000000000, 0.000000000000000000, -1.000000000000000000 ) ) ;
#8775 = LINE ( 'NONE', #10918, #10905 ) ;
#8776 = AXIS2_PLACEMENT_3D ( 'NONE', #9258, #533, #9400 ) ;
#8777 = EDGE_LOOP ( 'NONE', ( #8867, #5223 ) ) ;
#8778 = CARTESIAN_POINT ( 'NONE',  ( 629.0000000000000000, 154.0000000000000284, -187.5000000000000000 ) ) ;
#8779 = ORIENTED_EDGE ( 'NONE', *, *, #1577, .T. ) ;
#8780 = VECTOR ( 'NONE', #12260, 1000.000000000000000 ) ;
#8781 = ORIENTED_EDGE ( 'NONE', *, *, #13561, .F. ) ;
#8782 = CARTESIAN_POINT ( 'NONE',  ( 1.399999999999998579, 9.184850993605147944E-16, 7.500000000000000000 ) ) ;
#8783 = CARTESIAN_POINT ( 'NONE',  ( 650.0000000000000000, 175.0000000000000568, -210.0000000000000000 ) ) ;
#8784 = VECTOR ( 'NONE', #13641, 1000.000000000000114 ) ;
#8785 = CARTESIAN_POINT ( 'NONE',  ( 631.0000000000000000, 155.9999999999999432, -233.5000000000000000 ) ) ;
#8786 = EDGE_CURVE ( 'NONE', #13261, #11130, #2400, .T. ) ;
#8787 = CARTESIAN_POINT ( 'NONE',  ( 635.0000000000000000, 160.0000000000000284, 215.5000000000000000 ) ) ;
#8788 = CARTESIAN_POINT ( 'NONE',  ( 636.9746078850427011, 155.6249658629529620, -210.0000000000000000 ) ) ;
#8789 = DIRECTION ( 'NONE',  ( 0.000000000000000000, -0.4999999999999990563, 0.8660254037844391517 ) ) ;
#8790 = VERTEX_POINT ( 'NONE', #10227 ) ;
#8791 = DIRECTION ( 'NONE',  ( 1.000000000000000000, 0.000000000000000000, 0.000000000000000000 ) ) ;
#8792 = LINE ( 'NONE', #582, #12221 ) ;
#8793 = PRODUCT_CONTEXT ( 'NONE', #9611, 'mechanical' ) ;
#8794 = AXIS2_PLACEMENT_3D ( 'NONE', #11988, #12135, #4253 ) ;
#8795 = DIRECTION ( 'NONE',  ( -1.000000000000000000, -0.000000000000000000, -0.000000000000000000 ) ) ;
#8796 = ORIENTED_EDGE ( 'NONE', *, *, #1966, .T. ) ;
#8797 = VERTEX_POINT ( 'NONE', #8004 ) ;
#8798 = CARTESIAN_POINT ( 'NONE',  ( 446.3084422793565409, 264.0194060144110608, -187.0000000000000000 ) ) ;
#8799 = CARTESIAN_POINT ( 'NONE',  ( -4.358513833876417998, -4.989164364209884184, -0.07763482564821273801 ) ) ;
#8800 = DIRECTION ( 'NONE',  ( 0.000000000000000000, 0.8660254037844380415, -0.5000000000000012212 ) ) ;
#8801 = ADVANCED_FACE ( 'NONE', ( #11542 ), #11188, .F. ) ;
#8802 = CARTESIAN_POINT ( 'NONE',  ( 1.127757440534757238, 7.231345287187090243, -6.344532336093706704 ) ) ;
#8803 = ORIENTED_EDGE ( 'NONE', *, *, #3391, .F. ) ;
#8804 = CARTESIAN_POINT ( 'NONE',  ( -6.815962252199548210, 1.383413844627830791, -6.173425845474762141 ) ) ;
#8805 = VERTEX_POINT ( 'NONE', #85 ) ;
#8806 = DIRECTION ( 'NONE',  ( 2.985317128751799872E-15, 6.087367539060727577E-15, -1.000000000000000000 ) ) ;
#8807 = DIRECTION ( 'NONE',  ( -0.9578262852211517631, 0.2873478855663442189, 4.622231866529365347E-30 ) ) ;
#8808 = DIRECTION ( 'NONE',  ( 0.000000000000000000, -1.000000000000000000, 0.000000000000000000 ) ) ;
#8809 = FILL_AREA_STYLE ('',( #9624 ) ) ;
#8810 = B_SPLINE_CURVE_WITH_KNOTS ( 'NONE', 3,
 ( #6480, #14583, #7661, #13483 ),
 .UNSPECIFIED., .F., .F.,
 ( 4, 4 ),
 ( 2.380735203086576123E-07, 0.002921158011986709890 ),
 .UNSPECIFIED. ) ;
#8811 = ORIENTED_EDGE ( 'NONE', *, *, #13505, .T. ) ;
#8812 = EDGE_CURVE ( 'NONE', #9079, #5147, #12507, .T. ) ;
#8813 = FACE_OUTER_BOUND ( 'NONE', #10460, .T. ) ;
#8814 = ORIENTED_EDGE ( 'NONE', *, *, #13790, .T. ) ;
#8815 = ORIENTED_EDGE ( 'NONE', *, *, #9821, .T. ) ;
#8816 = CARTESIAN_POINT ( 'NONE',  ( 635.0000000000000000, 160.0000000000000284, -233.5000000000000000 ) ) ;
#8817 = EDGE_CURVE ( 'NONE', #7390, #11788, #4510, .T. ) ;
#8818 = FACE_OUTER_BOUND ( 'NONE', #7718, .T. ) ;
#8819 = DIRECTION ( 'NONE',  ( 0.000000000000000000, -1.000000000000000000, 0.000000000000000000 ) ) ;
#8820 = VERTEX_POINT ( 'NONE', #3598 ) ;
#8821 = EDGE_LOOP ( 'NONE', ( #1168, #4845, #9291, #5840 ) ) ;
#8822 = LINE ( 'NONE', #13174, #7595 ) ;
#8823 = CARTESIAN_POINT ( 'NONE',  ( 2.000000000000008882, 3.464101615137749945, 0.000000000000000000 ) ) ;
#8824 = CARTESIAN_POINT ( 'NONE',  ( 455.5035746174796714, 294.6698471414878782, -210.0000000000000000 ) ) ;
#8825 = DIRECTION ( 'NONE',  ( 0.000000000000000000, 0.000000000000000000, 1.000000000000000000 ) ) ;
#8826 = CARTESIAN_POINT ( 'NONE',  ( 650.0000000000000000, 145.0000000000000568, 210.0000000000000000 ) ) ;
#8827 = ORIENTED_EDGE ( 'NONE', *, *, #12968, .T. ) ;
#8828 = EDGE_CURVE ( 'NONE', #151, #12920, #9460, .T. ) ;
#8829 = PRESENTATION_STYLE_ASSIGNMENT (( #14508 ) ) ;
#8830 = CONTEXT_DEPENDENT_SHAPE_REPRESENTATION ( #1421, #2540 ) ;
#8831 = ORIENTED_EDGE ( 'NONE', *, *, #4768, .T. ) ;
#8832 = LINE ( 'NONE', #3001, #13704 ) ;
#8833 = EDGE_CURVE ( 'NONE', #9217, #3430, #12358, .T. ) ;
#8834 = ORIENTED_EDGE ( 'NONE', *, *, #7565, .T. ) ;
#8835 = DIRECTION ( 'NONE',  ( -0.000000000000000000, -0.000000000000000000, -1.000000000000000000 ) ) ;
#8836 = CARTESIAN_POINT ( 'NONE',  ( 636.7717819724297215, 155.3244477714206653, -210.0000000000000000 ) ) ;
#8837 = VERTEX_POINT ( 'NONE', #4471 ) ;
#8838 = DIRECTION ( 'NONE',  ( 0.000000000000000000, 0.000000000000000000, -1.000000000000000000 ) ) ;
#8839 = DIRECTION ( 'NONE',  ( 0.000000000000000000, -0.4999999999999993339, 0.8660254037844390407 ) ) ;
#8840 = CARTESIAN_POINT ( 'NONE',  ( 43.50000000000000711, 0.000000000000000000, 0.000000000000000000 ) ) ;
#8841 = ORIENTED_EDGE ( 'NONE', *, *, #10128, .F. ) ;
#8842 = CARTESIAN_POINT ( 'NONE',  ( 707.5067158355134325, 162.6912496279593370, -179.7999999999999261 ) ) ;
#8843 = ORIENTED_EDGE ( 'NONE', *, *, #5426, .T. ) ;
#8844 = ORIENTED_EDGE ( 'NONE', *, *, #1769, .T. ) ;
#8845 = CARTESIAN_POINT ( 'NONE',  ( 451.3035746174797396, 294.6698471414878782, -190.0000000000000568 ) ) ;
#8846 = DIRECTION ( 'NONE',  ( 0.000000000000000000, 0.000000000000000000, -1.000000000000000000 ) ) ;
#8847 = FACE_OUTER_BOUND ( 'NONE', #5780, .T. ) ;
#8848 = EDGE_CURVE ( 'NONE', #5092, #1005, #239, .T. ) ;
#8849 = CARTESIAN_POINT ( 'NONE',  ( 0.000000000000000000, -2.357898499370432166, 3.035766082959412415E-15 ) ) ;
#8850 = EDGE_CURVE ( 'NONE', #13374, #2544, #5684, .T. ) ;
#8851 = CARTESIAN_POINT ( 'NONE',  ( 2.241046694639346804, 6.576374040526301812, -6.171384342982712212 ) ) ;
#8852 = CARTESIAN_POINT ( 'NONE',  ( 703.1581845006096501, 166.2926764603917036, -177.6000000000005059 ) ) ;
#8853 = CARTESIAN_POINT ( 'NONE',  ( -6.831979103402614051, -3.295157223185839701, -6.443785395948805395 ) ) ;
#8854 = APPLICATION_CONTEXT ( 'automotive_design' ) ;
#8855 = VERTEX_POINT ( 'NONE', #8219 ) ;
#8856 = CARTESIAN_POINT ( 'NONE',  ( -8.505790995054995918, 418.4210031920607662, -187.0000000000000000 ) ) ;
#8857 = CARTESIAN_POINT ( 'NONE',  ( 6.506987859255522366, -5.850751062354595078, -3.430629538771514681E-16 ) ) ;
#8858 = PRODUCT_CONTEXT ( 'NONE', #12344, 'mechanical' ) ;
#8859 = CARTESIAN_POINT ( 'NONE',  ( 0.000000000000000000, 0.000000000000000000, 0.000000000000000000 ) ) ;
#8860 = ORIENTED_EDGE ( 'NONE', *, *, #5304, .T. ) ;
#8861 = ORIENTED_EDGE ( 'NONE', *, *, #5834, .T. ) ;
#8862 =( LENGTH_UNIT ( ) NAMED_UNIT ( * ) SI_UNIT ( .MILLI., .METRE. ) );
#8863 = DIRECTION ( 'NONE',  ( 0.000000000000000000, 0.000000000000000000, -1.000000000000000000 ) ) ;
#8864 = EDGE_CURVE ( 'NONE', #2268, #9217, #6011, .T. ) ;
#8865 = PLANE ( 'NONE',  #8705 ) ;
#8866 = CARTESIAN_POINT ( 'NONE',  ( 130.2060951089102332, 434.0203170297008910, 190.0000000000001990 ) ) ;
#8867 = ORIENTED_EDGE ( 'NONE', *, *, #6080, .F. ) ;
#8868 = DIRECTION ( 'NONE',  ( 0.000000000000000000, 1.000000000000000000, 0.000000000000000000 ) ) ;
#8869 = ORIENTED_EDGE ( 'NONE', *, *, #5426, .F. ) ;
#8870 = DIRECTION ( 'NONE',  ( -0.2873478855663502141, -0.9578262852211498757, 0.000000000000000000 ) ) ;
#8871 = CARTESIAN_POINT ( 'NONE',  ( 448.9584422793565750, 264.0194060144110608, -190.0000000000000000 ) ) ;
#8872 = CARTESIAN_POINT ( 'NONE',  ( 705.2654023280958882, 165.6605111121457981, 177.6000000000001648 ) ) ;
#8873 = VERTEX_POINT ( 'NONE', #10450 ) ;
#8874 = ORIENTED_EDGE ( 'NONE', *, *, #7446, .F. ) ;
#8875 = CARTESIAN_POINT ( 'NONE',  ( -4.000000000000000000, 2.309401076758498483, -3.433295621305379353 ) ) ;
#8876 = EDGE_CURVE ( 'NONE', #1729, #197, #2920, .T. ) ;
#8877 = PLANE ( 'NONE',  #5402 ) ;
#8878 = CARTESIAN_POINT ( 'NONE',  ( -2.855764796983342624, 2.970025579236414082, -0.09382832055445475272 ) ) ;
#8879 = ORIENTED_EDGE ( 'NONE', *, *, #12581, .T. ) ;
#8880 = VERTEX_POINT ( 'NONE', #10736 ) ;
#8881 = DIRECTION ( 'NONE',  ( 0.000000000000000000, 0.000000000000000000, -1.000000000000000000 ) ) ;
#8882 = CARTESIAN_POINT ( 'NONE',  ( 2.500000000000000000, 0.000000000000000000, 0.000000000000000000 ) ) ;
#8883 = DIRECTION ( 'NONE',  ( -1.000000000000000000, 0.000000000000000000, 0.000000000000000000 ) ) ;
#8884 = FACE_OUTER_BOUND ( 'NONE', #914, .T. ) ;
#8885 = CARTESIAN_POINT ( 'NONE',  ( -10.00000000000000000, 413.4403065089105667, -210.0000000000000000 ) ) ;
#8886 = ORIENTED_EDGE ( 'NONE', *, *, #3902, .F. ) ;
#8887 = CARTESIAN_POINT ( 'NONE',  ( 609.7735223591643035, 188.7684563956151464, 189.4730470240896807 ) ) ;
#8888 = ORIENTED_EDGE ( 'NONE', *, *, #12305, .F. ) ;
#8889 = ORIENTED_EDGE ( 'NONE', *, *, #10418, .T. ) ;
#8890 = CARTESIAN_POINT ( 'NONE',  ( -4.078421086530219064, -3.990950201428956845, -1.000000000000000000 ) ) ;
#8891 = EDGE_CURVE ( 'NONE', #8139, #7944, #9563, .T. ) ;
#8892 = VERTEX_POINT ( 'NONE', #12949 ) ;
#8893 = VECTOR ( 'NONE', #6098, 1000.000000000000000 ) ;
#8894 = EDGE_CURVE ( 'NONE', #11836, #2008, #13835, .T. ) ;
#8895 = CARTESIAN_POINT ( 'NONE',  ( 0.000000000000000000, 0.5192545390863916310, -1.000000000000000000 ) ) ;
#8896 = ADVANCED_FACE ( 'NONE', ( #4026 ), #7263, .F. ) ;
#8897 = CARTESIAN_POINT ( 'NONE',  ( 137.1540310085880776, 355.9707293956415697, 187.0000000000000000 ) ) ;
#8898 = EDGE_CURVE ( 'NONE', #1513, #10237, #8368, .T. ) ;
#8899 = ORIENTED_EDGE ( 'NONE', *, *, #10343, .T. ) ;
#8900 = DIRECTION ( 'NONE',  ( 0.000000000000000000, 0.000000000000000000, 1.000000000000000000 ) ) ;
#8901 = DIRECTION ( 'NONE',  ( -1.000000000000000000, 0.000000000000000000, 0.000000000000000000 ) ) ;
#8902 = ADVANCED_FACE ( 'NONE', ( #14131 ), #1514, .F. ) ;
#8903 = AXIS2_PLACEMENT_3D ( 'NONE', #4774, #6005, #4988 ) ;
#8904 = FACE_BOUND ( 'NONE', #12121, .T. ) ;
#8905 = PLANE ( 'NONE',  #6437 ) ;
#8906 = SURFACE_SIDE_STYLE ('',( #14596 ) ) ;
#8907 = ORIENTED_EDGE ( 'NONE', *, *, #8467, .F. ) ;
#8908 = CARTESIAN_POINT ( 'NONE',  ( 451.3035746174797396, 294.6698471414878782, -187.0000000000000568 ) ) ;
#8909 = EDGE_CURVE ( 'NONE', #6858, #12823, #9630, .T. ) ;
#8910 = EDGE_LOOP ( 'NONE', ( #12875, #12589, #13916, #13725, #6126, #4068 ) ) ;
#8911 = ORIENTED_EDGE ( 'NONE', *, *, #6759, .T. ) ;
#8912 = CARTESIAN_POINT ( 'NONE',  ( 635.0000000000000000, 160.0000000000000284, -222.5000000000000000 ) ) ;
#8913 = AXIS2_PLACEMENT_3D ( 'NONE', #10764, #510, #4955 ) ;
#8914 = VECTOR ( 'NONE', #3788, 1000.000000000000000 ) ;
#8916 = VECTOR ( 'NONE', #13763, 1000.000000000000114 ) ;
#8915 = LINE ( 'NONE', #8783, #919 ) ;
#8917 = EDGE_CURVE ( 'NONE', #2870, #12209, #1575, .T. ) ;
#8918 = CARTESIAN_POINT ( 'NONE',  ( 1.393927851585479161, -4.043713361053543842, -3.526374918436840922 ) ) ;
#8919 = ADVANCED_FACE ( 'NONE', ( #12877 ), #1657, .T. ) ;
#8920 = CARTESIAN_POINT ( 'NONE',  ( 229.2257385731838326, 308.4724102386206255, 179.7999999999995850 ) ) ;
#8921 = CARTESIAN_POINT ( 'NONE',  ( -0.2813450144774468642, 7.667988119308851047, -6.122077150241852728 ) ) ;
#8922 = CARTESIAN_POINT ( 'NONE',  ( 635.0000000000000000, 160.0000000000000284, 215.5000000000000000 ) ) ;
#8923 = DIRECTION ( 'NONE',  ( -0.9578262852211508749, 0.2873478855663467724, 0.000000000000000000 ) ) ;
#8924 = ORIENTED_EDGE ( 'NONE', *, *, #10915, .F. ) ;
#8925 = VECTOR ( 'NONE', #5929, 1000.000000000000114 ) ;
#8926 = AXIS2_PLACEMENT_3D ( 'NONE', #2997, #13182, #1967 ) ;
#8927 = DIRECTION ( 'NONE',  ( 1.000000000000000000, 0.000000000000000000, 0.000000000000000000 ) ) ;
#8928 = CARTESIAN_POINT ( 'NONE',  ( 642.0000000000000000, 153.0000000000000284, -233.5000000000000000 ) ) ;
#8929 = DIRECTION ( 'NONE',  ( 1.000000000000000000, 0.000000000000000000, -0.000000000000000000 ) ) ;
#8930 = EDGE_CURVE ( 'NONE', #1538, #8790, #6168, .T. ) ;
#8931 = ORIENTED_EDGE ( 'NONE', *, *, #7197, .F. ) ;
#8932 = ORIENTED_EDGE ( 'NONE', *, *, #14023, .F. ) ;
#8933 = DIRECTION ( 'NONE',  ( -0.9237280213470676626, -0.3830490080632388272, 0.000000000000000000 ) ) ;
#8934 = AXIS2_PLACEMENT_3D ( 'NONE', #10476, #1256, #5489 ) ;
#8935 = EDGE_CURVE ( 'NONE', #9718, #5667, #13470, .T. ) ;
#8936 = CYLINDRICAL_SURFACE ( 'NONE', #676, 2.649999999999985700 ) ;
#8937 = VECTOR ( 'NONE', #11135, 1000.000000000000000 ) ;
#8938 = VECTOR ( 'NONE', #12026, 1000.000000000000000 ) ;
#8939 = CARTESIAN_POINT ( 'NONE',  ( 2.999999999999999112, 2.309401076758500704, -4.000000000000000000 ) ) ;
#8940 = ORIENTED_EDGE ( 'NONE', *, *, #13201, .F. ) ;
#8941 = CARTESIAN_POINT ( 'NONE',  ( 0.000000000000000000, 0.000000000000000000, 0.000000000000000000 ) ) ;
#8942 = ORIENTED_EDGE ( 'NONE', *, *, #2072, .T. ) ;
#8943 = DIRECTION ( 'NONE',  ( -1.000000000000000000, 0.000000000000000000, 0.000000000000000000 ) ) ;
#8944 = DIRECTION ( 'NONE',  ( -0.000000000000000000, -0.000000000000000000, -1.000000000000000000 ) ) ;
#8945 =( NAMED_UNIT ( * ) SI_UNIT ( $, .STERADIAN. ) SOLID_ANGLE_UNIT ( ) );
#8946 = VECTOR ( 'NONE', #6411, 1000.000000000000000 ) ;
#8947 = CARTESIAN_POINT ( 'NONE',  ( 0.4465819873852032162, 5.773502691896260863, 3.074436065535979155E-16 ) ) ;
#8948 = AXIS2_PLACEMENT_3D ( 'NONE', #11340, #4483, #14520 ) ;
#8949 = ORIENTED_EDGE ( 'NONE', *, *, #7887, .F. ) ;
#8950 = ORIENTED_EDGE ( 'NONE', *, *, #6995, .T. ) ;
#8951 = DIRECTION ( 'NONE',  ( -0.000000000000000000, -0.000000000000000000, 1.000000000000000000 ) ) ;
#8952 = DIRECTION ( 'NONE',  ( -1.000000000000000000, 0.000000000000000000, 0.000000000000000000 ) ) ;
#8953 = AXIS2_PLACEMENT_3D ( 'NONE', #1950, #7482, #11974 ) ;
#8954 = TOROIDAL_SURFACE ( 'NONE', #2594, 6.250000000000000000, 0.7500000000000000000 ) ;
#8955 = CARTESIAN_POINT ( 'NONE',  ( 440.1783540539411774, 278.3868002927282532, -210.0000000000000000 ) ) ;
#8956 = AXIS2_PLACEMENT_3D ( 'NONE', #13035, #4917, #7419 ) ;
#8957 = EDGE_LOOP ( 'NONE', ( #7646, #8464, #1678, #10892, #6604, #13465, #8364 ) ) ;
#8958 = VECTOR ( 'NONE', #13042, 1000.000000000000114 ) ;
#8959 = ORIENTED_EDGE ( 'NONE', *, *, #8006, .F. ) ;
#8960 = DIRECTION ( 'NONE',  ( 0.000000000000000000, 0.000000000000000000, -1.000000000000000000 ) ) ;
#8961 = EDGE_CURVE ( 'NONE', #13374, #2766, #14062, .T. ) ;
#8962 = CARTESIAN_POINT ( 'NONE',  ( 3.700000000000000178, 0.000000000000000000, -2.700000000000000622 ) ) ;
#8963 = CARTESIAN_POINT ( 'NONE',  ( 7.900000000000002132, 0.000000000000000000, 0.000000000000000000 ) ) ;
#8964 = DIRECTION ( 'NONE',  ( -0.000000000000000000, -0.000000000000000000, -1.000000000000000000 ) ) ;
#8965 = CARTESIAN_POINT ( 'NONE',  ( 0.1391502195351252413, -2.687187980154734923, -3.345653888883608040 ) ) ;
#8966 = SHAPE_REPRESENTATION_RELATIONSHIP ( 'NONE' , 'NONE' ,  #5933, #4208 ) ;
#8967 = VECTOR ( 'NONE', #3253, 1000.000000000000000 ) ;
#8968 = ORIENTED_EDGE ( 'NONE', *, *, #12194, .F. ) ;
#8969 = VECTOR ( 'NONE', #7685, 1000.000000000000000 ) ;
#8970 = DIRECTION ( 'NONE',  ( 1.000000000000000000, 0.000000000000000000, 0.000000000000000000 ) ) ;
#8971 = ORIENTED_EDGE ( 'NONE', *, *, #4126, .F. ) ;
#8972 = VERTEX_POINT ( 'NONE', #6085 ) ;
#8973 = DIRECTION ( 'NONE',  ( -0.000000000000000000, -0.000000000000000000, -1.000000000000000000 ) ) ;
#8974 = VECTOR ( 'NONE', #7568, 1000.000000000000000 ) ;
#8975 = VECTOR ( 'NONE', #335, 1000.000000000000000 ) ;
#8976 = VERTEX_POINT ( 'NONE', #10587 ) ;
#8977 = DIRECTION ( 'NONE',  ( 0.000000000000000000, 0.000000000000000000, -1.000000000000000000 ) ) ;
#8978 = VECTOR ( 'NONE', #6793, 1000.000000000000114 ) ;
#8979 = VECTOR ( 'NONE', #1293, 999.9999999999998863 ) ;
#8980 = DIRECTION ( 'NONE',  ( -1.000000000000000000, -0.000000000000000000, -0.000000000000000000 ) ) ;
#8981 = ORIENTED_EDGE ( 'NONE', *, *, #13418, .F. ) ;
#8982 = CARTESIAN_POINT ( 'NONE',  ( 2.999999999999999112, 4.000000000000000000, 0.000000000000000000 ) ) ;
#8983 = EDGE_CURVE ( 'NONE', #10969, #2440, #765, .T. ) ;
#8984 = CARTESIAN_POINT ( 'NONE',  ( 0.000000000000000000, 0.000000000000000000, -190.0000000000000000 ) ) ;
#8985 = AXIS2_PLACEMENT_3D ( 'NONE', #6030, #3682, #7215 ) ;
#8986 = DIRECTION ( 'NONE',  ( -1.000000000000000000, 0.000000000000000000, 0.000000000000000000 ) ) ;
#8987 = ORIENTED_EDGE ( 'NONE', *, *, #6073, .T. ) ;
#8988 = EDGE_CURVE ( 'NONE', #3959, #2398, #11903, .T. ) ;
#8989 = CYLINDRICAL_SURFACE ( 'NONE', #14605, 4.000000000000000000 ) ;
#8990 = ORIENTED_EDGE ( 'NONE', *, *, #2401, .F. ) ;
#8991 = AXIS2_PLACEMENT_3D ( 'NONE', #3840, #566, #10753 ) ;
#8992 = VECTOR ( 'NONE', #7318, 1000.000000000000227 ) ;
#8993 = EDGE_CURVE ( 'NONE', #2816, #1012, #1448, .T. ) ;
#8994 = ORIENTED_EDGE ( 'NONE', *, *, #853, .F. ) ;
#8995 = FACE_OUTER_BOUND ( 'NONE', #5022, .T. ) ;
#8996 = EDGE_CURVE ( 'NONE', #2224, #1897, #5927, .T. ) ;
#8997 = CARTESIAN_POINT ( 'NONE',  ( -1.500000000000000888, 6.245698675651501825E-16, 5.100000000000000533 ) ) ;
#8998 = CARTESIAN_POINT ( 'NONE',  ( 4.000000000000000000, -1.560351142792952617, -0.2242961665059816367 ) ) ;
#8999 = VECTOR ( 'NONE', #4788, 1000.000000000000000 ) ;
#9000 = CARTESIAN_POINT ( 'NONE',  ( 708.1388811837590538, 164.7984674554467404, 179.7999999999995850 ) ) ;
#9001 = DIRECTION ( 'NONE',  ( -1.000000000000000000, 0.000000000000000000, 0.000000000000000000 ) ) ;
#9002 = PLANE ( 'NONE',  #2842 ) ;
#9003 = FACE_OUTER_BOUND ( 'NONE', #1240, .T. ) ;
#9004 = ORIENTED_EDGE ( 'NONE', *, *, #472, .T. ) ;
#9005 = PRESENTATION_LAYER_ASSIGNMENT (  '', '', ( #6875 ) ) ;
#9006 = CARTESIAN_POINT ( 'NONE',  ( 610.0000000000001137, 185.6790804732684705, -184.8000000000000398 ) ) ;
#9007 = CARTESIAN_POINT ( 'NONE',  ( 6.355827204229364646, -3.436818823786764732, -4.264647808192652434 ) ) ;
#9008 = APPLICATION_PROTOCOL_DEFINITION ( 'draft international standard', 'automotive_design', 1998, #3296 ) ;
#9009 = EDGE_CURVE ( 'NONE', #11318, #2694, #7704, .T. ) ;
#9010 = EDGE_CURVE ( 'NONE', #9101, #12192, #10172, .T. ) ;
#9011 = DIRECTION ( 'NONE',  ( 1.000000000000000000, 0.000000000000000000, 0.000000000000000000 ) ) ;
#9012 = ORIENTED_EDGE ( 'NONE', *, *, #4856, .T. ) ;
#9013 = ORIENTED_EDGE ( 'NONE', *, *, #4448, .F. ) ;
#9014 = CIRCLE ( 'NONE', #6656, 3.309499999999999886 ) ;
#9015 = CARTESIAN_POINT ( 'NONE',  ( 5.991014884144047592, 4.330127018922190096, -2.500000000000003997 ) ) ;
#9016 = EDGE_CURVE ( 'NONE', #7459, #10586, #2175, .T. ) ;
#9017 = DIRECTION ( 'NONE',  ( 0.000000000000000000, 0.5000000000000011102, 0.8660254037844379305 ) ) ;
#9018 = AXIS2_PLACEMENT_3D ( 'NONE', #10666, #4369, #8863 ) ;
#9019 = CARTESIAN_POINT ( 'NONE',  ( 6.837824896291514243, 3.947820044545427454, -6.564402953523716278 ) ) ;
#9020 = VECTOR ( 'NONE', #8603, 1000.000000000000000 ) ;
#9021 = FACE_OUTER_BOUND ( 'NONE', #3360, .T. ) ;
#9022 = ORIENTED_EDGE ( 'NONE', *, *, #3792, .F. ) ;
#9023 = CARTESIAN_POINT ( 'NONE',  ( 6.355324643801637308, 1.972141403783279623, -5.108685331087993831 ) ) ;
#9024 = CARTESIAN_POINT ( 'NONE',  ( 7.240873133980779919, 470.9098836221796773, 187.0000000000001990 ) ) ;
#9025 =( NAMED_UNIT ( * ) PLANE_ANGLE_UNIT ( ) SI_UNIT ( $, .RADIAN. ) );
#9026 = DIRECTION ( 'NONE',  ( 0.000000000000000000, 0.000000000000000000, -1.000000000000000000 ) ) ;
#9027 = ORIENTED_EDGE ( 'NONE', *, *, #7379, .T. ) ;
#9028 = ORIENTED_EDGE ( 'NONE', *, *, #493, .F. ) ;
#9029 = DIRECTION ( 'NONE',  ( 0.000000000000000000, 0.000000000000000000, -1.000000000000000000 ) ) ;
#9030 = LINE ( 'NONE', #12483, #662 ) ;
#9031 = AXIS2_PLACEMENT_3D ( 'NONE', #7427, #9788, #10002 ) ;
#9032 = CARTESIAN_POINT ( 'NONE',  ( 4.000000000000000000, -1.677850389431204459, -3.535268758346977513 ) ) ;
#9033 =( BOUNDED_SURFACE ( )  B_SPLINE_SURFACE ( 3, 2, ( 
 ( #10598, #5008, #13844 ),
 ( #9571, #2638, #14071 ),
 ( #2851, #8151, #11846 ),
 ( #4790, #12658, #6021 ),
 ( #1960, #9787, #7652 ),
 ( #7575, #773, #14146 ) ),
 .UNSPECIFIED., .F., .F., .F. ) 
 B_SPLINE_SURFACE_WITH_KNOTS ( ( 4, 2, 4 ),
 ( 3, 3 ),
 ( 0.02032853247518126918, 0.02278863295364821906, 0.02524873343211516893 ),
 ( 0.000000000000000000, 1.000000000000000000 ),
 .UNSPECIFIED. ) 
 GEOMETRIC_REPRESENTATION_ITEM ( )  RATIONAL_B_SPLINE_SURFACE ( (
 ( 1.000000000000000000, 0.8047781615896838492, 1.000000000000000000),
 ( 1.000000000000000000, 0.8123767586288186404, 1.000000000000000000),
 ( 1.000000000000000000, 0.8190662415565814758, 1.000000000000000000),
 ( 1.000000000000000000, 0.8192361015667604107, 1.000000000000000000),
 ( 1.000000000000000000, 0.8126135807104967190, 1.000000000000000000),
 ( 1.000000000000000000, 0.8047712338318580017, 1.000000000000000000) ) ) 
 REPRESENTATION_ITEM ( '' )  SURFACE ( )  );
#9034 = ORIENTED_EDGE ( 'NONE', *, *, #2021, .T. ) ;
#9035 = DIRECTION ( 'NONE',  ( -0.9578262852211513190, 0.2873478855663453846, 0.000000000000000000 ) ) ;
#9036 = CARTESIAN_POINT ( 'NONE',  ( 609.8556724072889210, 189.7221213180926611, -189.8938770989753095 ) ) ;
#9037 = DIRECTION ( 'NONE',  ( 1.000000000000000000, 0.000000000000000000, 0.000000000000000000 ) ) ;
#9038 = B_SPLINE_CURVE_WITH_KNOTS ( 'NONE', 3,
 ( #2119, #9963, #8998, #6708, #1161, #3454 ),
 .UNSPECIFIED., .F., .F.,
 ( 4, 2, 4 ),
 ( 0.003358874760055551890, 0.004541967308452098118, 0.005725059856848645212 ),
 .UNSPECIFIED. ) ;
#9039 = CARTESIAN_POINT ( 'NONE',  ( 6.500000000000000000, 3.752776749732563921, -6.064240316920399110 ) ) ;
#9040 = DIRECTION ( 'NONE',  ( 0.000000000000000000, -0.4999999999999993339, 0.8660254037844390407 ) ) ;
#9041 = FACE_OUTER_BOUND ( 'NONE', #8910, .T. ) ;
#9042 = ORIENTED_EDGE ( 'NONE', *, *, #11509, .F. ) ;
#9043 = CARTESIAN_POINT ( 'NONE',  ( 446.3084422793565409, 264.0194060144110608, -190.0000000000000000 ) ) ;
#9044 = ORIENTED_EDGE ( 'NONE', *, *, #3411, .F. ) ;
#9045 = ORIENTED_EDGE ( 'NONE', *, *, #12054, .F. ) ;
#9046 = B_SPLINE_CURVE_WITH_KNOTS ( 'NONE', 3,
 ( #7775, #9165, #4534, #11165 ),
 .UNSPECIFIED., .F., .F.,
 ( 4, 4 ),
 ( 0.002977824986803825295, 0.005972417098209346735 ),
 .UNSPECIFIED. ) ;
#9047 = CARTESIAN_POINT ( 'NONE',  ( 7.240873133980779919, 470.9098836221796773, 187.0000000000001990 ) ) ;
#9048 = VERTEX_POINT ( 'NONE', #1796 ) ;
#9049 = EDGE_CURVE ( 'NONE', #852, #8674, #10887, .T. ) ;
#9050 = EDGE_CURVE ( 'NONE', #2847, #145, #12187, .T. ) ;
#9051 = CARTESIAN_POINT ( 'NONE',  ( -1.250000000000000000, -6.429618962271402616, 0.000000000000000000 ) ) ;
#9052 =( REPRESENTATION_RELATIONSHIP ('NONE','NONE', #2822, #342 ) REPRESENTATION_RELATIONSHIP_WITH_TRANSFORMATION ( #8455 )SHAPE_REPRESENTATION_RELATIONSHIP( ) );
#9053 = CARTESIAN_POINT ( 'NONE',  ( 2.500000000000000000, 0.000000000000000000, 0.000000000000000000 ) ) ;
#9054 = VERTEX_POINT ( 'NONE', #6300 ) ;
#9055 = CARTESIAN_POINT ( 'NONE',  ( 0.000000000000000000, 0.000000000000000000, 0.000000000000000000 ) ) ;
#9056 = CARTESIAN_POINT ( 'NONE',  ( 0.000000000000000000, -3.464101615137750834, 2.000000000000007994 ) ) ;
#9057 = CARTESIAN_POINT ( 'NONE',  ( -3.250000000000003997, -5.629165124598849879, 0.000000000000000000 ) ) ;
#9058 = CYLINDRICAL_SURFACE ( 'NONE', #4792, 5.000000000000000000 ) ;
#9059 = SURFACE_STYLE_USAGE ( .BOTH. , #12369 ) ;
#9060 = ORIENTED_EDGE ( 'NONE', *, *, #10355, .T. ) ;
#9061 = CARTESIAN_POINT ( 'NONE',  ( 3.500000000000000000, -4.618802153516999631, 0.000000000000000000 ) ) ;
#9062 = ORIENTED_EDGE ( 'NONE', *, *, #3792, .T. ) ;
#9063 = ORIENTED_EDGE ( 'NONE', *, *, #9009, .T. ) ;
#9064 = CARTESIAN_POINT ( 'NONE',  ( 10.00000000000000000, 10.00000000000000178, 210.0000000000000000 ) ) ;
#9065 = EDGE_CURVE ( 'NONE', #11130, #9710, #8281, .T. ) ;
#9066 = DIRECTION ( 'NONE',  ( 0.000000000000000000, 0.000000000000000000, -1.000000000000000000 ) ) ;
#9067 = CARTESIAN_POINT ( 'NONE',  ( 0.6937372685066666156, -4.453844082567737672, -3.610536846335894445 ) ) ;
#9068 = DIRECTION ( 'NONE',  ( -0.000000000000000000, -0.000000000000000000, 1.000000000000000000 ) ) ;
#9069 = EDGE_CURVE ( 'NONE', #14470, #3740, #695, .T. ) ;
#9070 = CARTESIAN_POINT ( 'NONE',  ( 708.1388811837593948, 164.7984674554473088, 179.8000000000001819 ) ) ;
#9071 = DIRECTION ( 'NONE',  ( 1.000000000000000000, -3.469446951953611033E-15, 0.000000000000000000 ) ) ;
#9072 = PLANE ( 'NONE',  #4176 ) ;
#9073 = ORIENTED_EDGE ( 'NONE', *, *, #3771, .F. ) ;
#9074 = DIRECTION ( 'NONE',  ( -1.000000000000000000, 0.000000000000000000, 0.000000000000000000 ) ) ;
#9075 = DIRECTION ( 'NONE',  ( 0.000000000000000000, 0.000000000000000000, 1.000000000000000000 ) ) ;
#9076 = DIRECTION ( 'NONE',  ( 1.148424442117026787E-15, -3.445273326351093279E-16, -1.000000000000000000 ) ) ;
#9077 = ORIENTED_EDGE ( 'NONE', *, *, #10389, .F. ) ;
#9078 = DIRECTION ( 'NONE',  ( 0.000000000000000000, 0.000000000000000000, 1.000000000000000000 ) ) ;
#9079 = VERTEX_POINT ( 'NONE', #682 ) ;
#9080 = VERTEX_POINT ( 'NONE', #1871 ) ;
#9081 = DIRECTION ( 'NONE',  ( 1.000000000000000000, 0.000000000000000000, 0.000000000000000000 ) ) ;
#9082 = CARTESIAN_POINT ( 'NONE',  ( 723.8855453127955570, 217.2873478855649694, -177.6000000000007617 ) ) ;
#9083 = ADVANCED_FACE ( 'NONE', ( #10803 ), #1173, .T. ) ;
#9084 = FACE_OUTER_BOUND ( 'NONE', #9223, .T. ) ;
#9085 = EDGE_CURVE ( 'NONE', #9145, #8805, #1208, .T. ) ;
#9086 = FACE_OUTER_BOUND ( 'NONE', #9304, .T. ) ;
#9087 = EDGE_CURVE ( 'NONE', #3684, #9769, #2985, .T. ) ;
#9088 = CARTESIAN_POINT ( 'NONE',  ( 6.390820841722130830, -2.823237767533158138, -5.110008744785250023 ) ) ;
#9089 = ORIENTED_EDGE ( 'NONE', *, *, #7209, .F. ) ;
#9090 = EDGE_CURVE ( 'NONE', #1630, #3851, #6057, .T. ) ;
#9091 = DIRECTION ( 'NONE',  ( 0.000000000000000000, 0.000000000000000000, -1.000000000000000000 ) ) ;
#9092 = CARTESIAN_POINT ( 'NONE',  ( -3.755786496842903988E-16, -7.505553499465146494, -6.064240316920404439 ) ) ;
#9093 = SURFACE_SIDE_STYLE ('',( #13592 ) ) ;
#9094 = CARTESIAN_POINT ( 'NONE',  ( 451.3035746174796827, 294.6698471414878782, 210.0000000000000000 ) ) ;
#9095 = VERTEX_POINT ( 'NONE', #14215 ) ;
#9096 = EDGE_LOOP ( 'NONE', ( #12427, #7876, #14342, #5180 ) ) ;
#9097 = CARTESIAN_POINT ( 'NONE',  ( 148.9991633467111569, 386.6211705227183870, -210.0000000000000000 ) ) ;
#9098 = DIRECTION ( 'NONE',  ( -0.9114654452181378819, -0.4113766427172328988, 0.000000000000000000 ) ) ;
#9099 = DIRECTION ( 'NONE',  ( 0.9578262852211507639, -0.2873478855663477716, -0.000000000000000000 ) ) ;
#9100 = ORIENTED_EDGE ( 'NONE', *, *, #7365, .F. ) ;
#9101 = VERTEX_POINT ( 'NONE', #2010 ) ;
#9102 = CARTESIAN_POINT ( 'NONE',  ( 610.0000000000001137, 191.1080398579019572, -187.0000000000000284 ) ) ;
#9103 = CARTESIAN_POINT ( 'NONE',  ( 4.799999999999999822, 0.000000000000000000, -1.000000000000000000 ) ) ;
#9104 = CARTESIAN_POINT ( 'NONE',  ( -4.141042297810615835, 2.227970268150415656, -3.687027686973619822 ) ) ;
#9105 = PLANE ( 'NONE',  #12428 ) ;
#9106 = DIRECTION ( 'NONE',  ( 0.000000000000000000, -0.8660254037844378194, 0.5000000000000014433 ) ) ;
#9107 = PRODUCT ( 'MAS-180', 'MAS-180', '', ( #5047 ) ) ;
#9108 = ORIENTED_EDGE ( 'NONE', *, *, #13201, .T. ) ;
#9109 = CARTESIAN_POINT ( 'NONE',  ( 707.5067158355133188, 162.6912496279604738, 177.6000000000001648 ) ) ;
#9110 = ORIENTED_EDGE ( 'NONE', *, *, #2541, .F. ) ;
#9111 = VERTEX_POINT ( 'NONE', #3060 ) ;
#9112 = DIRECTION ( 'NONE',  ( 1.000000000000000000, 0.000000000000000000, 0.000000000000000000 ) ) ;
#9113 = EDGE_CURVE ( 'NONE', #10478, #11861, #9, .T. ) ;
#9114 = VERTEX_POINT ( 'NONE', #6525 ) ;
#9115 = EDGE_CURVE ( 'NONE', #5721, #8820, #13100, .T. ) ;
#9116 = CARTESIAN_POINT ( 'NONE',  ( 630.0000000000000000, 160.0000000000000284, -187.5000000000000000 ) ) ;
#9117 = LINE ( 'NONE', #8011, #3004 ) ;
#9118 = ORIENTED_EDGE ( 'NONE', *, *, #583, .F. ) ;
#9119 = FACE_OUTER_BOUND ( 'NONE', #10866, .T. ) ;
#9120 = LINE ( 'NONE', #13489, #3057 ) ;
#9121 = CARTESIAN_POINT ( 'NONE',  ( 6.367873360227556567, 2.886751345948125547, 4.999999999999999112 ) ) ;
#9122 = CARTESIAN_POINT ( 'NONE',  ( 446.3084422793565409, 264.0194060144110608, 187.0000000000000000 ) ) ;
#9123 = ORIENTED_EDGE ( 'NONE', *, *, #9139, .F. ) ;
#9124 = VECTOR ( 'NONE', #3180, 1000.000000000000000 ) ;
#9125 = CYLINDRICAL_SURFACE ( 'NONE', #2097, 5.199999999999704414 ) ;
#9126 = AXIS2_PLACEMENT_3D ( 'NONE', #2923, #5210, #7199 ) ;
#9127 = ORIENTED_EDGE ( 'NONE', *, *, #3062, .T. ) ;
#9128 = ORIENTED_EDGE ( 'NONE', *, *, #10451, .T. ) ;
#9129 = DIRECTION ( 'NONE',  ( 0.000000000000000000, 0.000000000000000000, -1.000000000000000000 ) ) ;
#9130 = CARTESIAN_POINT ( 'NONE',  ( 639.6003227092664929, 153.9938615730590641, -210.0000000000000284 ) ) ;
#9131 = CARTESIAN_POINT ( 'NONE',  ( 611.4942090049448780, 232.4210031920607094, -187.0000000000000000 ) ) ;
#9132 = AXIS2_PLACEMENT_3D ( 'NONE', #11644, #7295, #11790 ) ;
#9133 = AXIS2_PLACEMENT_3D ( 'NONE', #614, #12065, #14287 ) ;
#9134 = FACE_OUTER_BOUND ( 'NONE', #2196, .T. ) ;
#9135 = EDGE_CURVE ( 'NONE', #11808, #10071, #3342, .T. ) ;
#9136 = DIRECTION ( 'NONE',  ( 1.000000000000000000, 0.000000000000000000, 0.000000000000000000 ) ) ;
#9137 = DIRECTION ( 'NONE',  ( -0.7071067811865364705, 8.659560562355067211E-17, -0.7071067811865584529 ) ) ;
#9138 = CARTESIAN_POINT ( 'NONE',  ( -4.799999999999999822, 5.878304635907294211E-16, -1.000000000000000000 ) ) ;
#9139 = EDGE_CURVE ( 'NONE', #4117, #12480, #2356, .T. ) ;
#9140 = ORIENTED_EDGE ( 'NONE', *, *, #14587, .F. ) ;
#9141 = DIRECTION ( 'NONE',  ( 0.2873478855663454401, 0.9578262852211513190, 0.000000000000000000 ) ) ;
#9142 = CARTESIAN_POINT ( 'NONE',  ( 8.500000000000000000, 0.000000000000000000, 7.900000000000002132 ) ) ;
#9143 = CARTESIAN_POINT ( 'NONE',  ( 610.2669374424701800, 189.5106555248625284, 186.4579326193729969 ) ) ;
#9144 = ITEM_DEFINED_TRANSFORMATION ( 'NONE', 'NONE', #1706,  #9440 ) ;
#9145 = VERTEX_POINT ( 'NONE', #3488 ) ;
#9146 = DIRECTION ( 'NONE',  ( -1.000000000000000000, 0.000000000000000000, 0.000000000000000000 ) ) ;
#9147 = VECTOR ( 'NONE', #5410, 1000.000000000000000 ) ;
#9148 = ORIENTED_EDGE ( 'NONE', *, *, #6109, .T. ) ;
#9149 = ORIENTED_EDGE ( 'NONE', *, *, #2675, .F. ) ;
#9150 = PRESENTATION_STYLE_ASSIGNMENT (( #1264 ) ) ;
#9151 = DIRECTION ( 'NONE',  ( -0.000000000000000000, -0.000000000000000000, 1.000000000000000000 ) ) ;
#9152 = CARTESIAN_POINT ( 'NONE',  ( 6.495567275914613248, -2.917443832165054207, 5.053160945538335724 ) ) ;
#9153 = CARTESIAN_POINT ( 'NONE',  ( 0.000000000000000000, 3.464101615137752610, 2.000000000000003997 ) ) ;
#9154 = CIRCLE ( 'NONE', #9865, 5.000000000000000000 ) ;
#9155 = VECTOR ( 'NONE', #868, 1000.000000000000000 ) ;
#9156 = UNCERTAINTY_MEASURE_WITH_UNIT (LENGTH_MEASURE( 1.000000000000000082E-05 ), #8453, 'distance_accuracy_value', 'NONE');
#9157 = DIRECTION ( 'NONE',  ( 1.000000000000000000, 0.000000000000000000, 0.000000000000000000 ) ) ;
#9158 = EDGE_CURVE ( 'NONE', #2314, #2790, #8341, .T. ) ;
#9159 = ORIENTED_EDGE ( 'NONE', *, *, #8988, .F. ) ;
#9160 = DIRECTION ( 'NONE',  ( -0.9578262852211524292, 0.2873478855663418874, 0.000000000000000000 ) ) ;
#9161 = DIRECTION ( 'NONE',  ( -0.000000000000000000, -0.000000000000000000, 1.000000000000000000 ) ) ;
#9162 = CARTESIAN_POINT ( 'NONE',  ( 635.0000000000000000, 160.0000000000000284, 210.0000000000000000 ) ) ;
#9163 = AXIS2_PLACEMENT_3D ( 'NONE', #12542, #2434, #12682 ) ;
#9164 = EDGE_CURVE ( 'NONE', #3628, #5994, #6872, .T. ) ;
#9165 = CARTESIAN_POINT ( 'NONE',  ( 6.244297270353400542, -0.9889575675955623035, 5.105276777067856209 ) ) ;
#9166 = ORIENTED_EDGE ( 'NONE', *, *, #11771, .F. ) ;
#9167 = ORIENTED_EDGE ( 'NONE', *, *, #4495, .F. ) ;
#9168 = CARTESIAN_POINT ( 'NONE',  ( 633.0368908673052601, 152.6952049249875927, 210.0000119999999981 ) ) ;
#9169 = CARTESIAN_POINT ( 'NONE',  ( 0.000000000000000000, 4.330127018922191873, 2.500000000000005773 ) ) ;
#9170 = AXIS2_PLACEMENT_3D ( 'NONE', #14077, #624, #13939 ) ;
#9171 = EDGE_CURVE ( 'NONE', #9848, #12715, #13460, .T. ) ;
#9172 = VECTOR ( 'NONE', #1626, 1000.000000000000000 ) ;
#9173 = DIRECTION ( 'NONE',  ( -0.000000000000000000, -0.000000000000000000, 1.000000000000000000 ) ) ;
#9174 = ADVANCED_FACE ( 'NONE', ( #3573 ), #12265, .F. ) ;
#9175 = CARTESIAN_POINT ( 'NONE',  ( 4.197310751797292738, 0.8178363989516252985, -3.502498386812444409 ) ) ;
#9176 = ORIENTED_EDGE ( 'NONE', *, *, #7901, .F. ) ;
#9177 = ORIENTED_EDGE ( 'NONE', *, *, #11085, .T. ) ;
#9178 = CARTESIAN_POINT ( 'NONE',  ( 609.7455576527837593, 188.4502455723027481, -189.3436892194421546 ) ) ;
#9179 = CARTESIAN_POINT ( 'NONE',  ( 145.1678582058265192, 408.6511750828049117, 210.0000000000000000 ) ) ;
#9180 = AXIS2_PLACEMENT_3D ( 'NONE', #5115, #1781, #5186 ) ;
#9181 = CARTESIAN_POINT ( 'NONE',  ( 6.533910050139697390, 5.901028503456122287, 2.527553615284464624E-14 ) ) ;
#9182 = CARTESIAN_POINT ( 'NONE',  ( -1.399999999999998579, 0.000000000000000000, -7.500000000000000000 ) ) ;
#9183 = CARTESIAN_POINT ( 'NONE',  ( 3.500000000000000000, 2.309401076758500704, -4.000000000000000000 ) ) ;
#9184 = ORIENTED_EDGE ( 'NONE', *, *, #11596, .F. ) ;
#9185 = DIRECTION ( 'NONE',  ( 1.000000000000000000, 0.000000000000000000, 0.000000000000000000 ) ) ;
#9186 = ORIENTED_EDGE ( 'NONE', *, *, #6399, .T. ) ;
#9187 = EDGE_LOOP ( 'NONE', ( #3388, #11185, #3928, #3662 ) ) ;
#9188 = CARTESIAN_POINT ( 'NONE',  ( 2.999999999999999112, -4.618802153516999631, 0.000000000000000000 ) ) ;
#9190 = ADVANCED_FACE ( 'NONE', ( #3649 ), #1278, .T. ) ;
#9189 = CIRCLE ( 'NONE', #9672, 2.199999999999685318 ) ;
#9191 = EDGE_CURVE ( 'NONE', #5769, #12523, #10133, .T. ) ;
#9192 = CIRCLE ( 'NONE', #1877, 5.249999999999976907 ) ;
#9193 = EDGE_CURVE ( 'NONE', #9351, #2694, #14182, .T. ) ;
#9194 = VECTOR ( 'NONE', #4460, 1000.000000000000114 ) ;
#9195 = LINE ( 'NONE', #7937, #3318 ) ;
#9196 = LINE ( 'NONE', #1517, #7241 ) ;
#9197 = VECTOR ( 'NONE', #3699, 1000.000000000000114 ) ;
#9198 = ORIENTED_EDGE ( 'NONE', *, *, #1515, .T. ) ;
#9199 = DIRECTION ( 'NONE',  ( 0.000000000000000000, 0.000000000000000000, -1.000000000000000000 ) ) ;
#9200 = CARTESIAN_POINT ( 'NONE',  ( 153.1991633467111456, 386.6211705227183870, 187.0000000000000568 ) ) ;
#9201 = VECTOR ( 'NONE', #9318, 1000.000000000000000 ) ;
#9202 = LINE ( 'NONE', #10086, #13133 ) ;
#9203 = CARTESIAN_POINT ( 'NONE',  ( 3.500000000000000000, 2.309401076758500704, -4.000000000000000000 ) ) ;
#9204 =( NAMED_UNIT ( * ) PLANE_ANGLE_UNIT ( ) SI_UNIT ( $, .RADIAN. ) );
#9205 = ORIENTED_EDGE ( 'NONE', *, *, #9433, .F. ) ;
#9206 = CIRCLE ( 'NONE', #4970, 0.2500000000000002220 ) ;
#9207 = TOROIDAL_SURFACE ( 'NONE', #2613, 7.900000000000002132, 0.5999999999999976463 ) ;
#9208 = CARTESIAN_POINT ( 'NONE',  ( 708.1388811837591675, 164.7984674554467119, 177.5999999999999091 ) ) ;
#9209 = ORIENTED_EDGE ( 'NONE', *, *, #1952, .F. ) ;
#9210 = EDGE_LOOP ( 'NONE', ( #13436, #5522, #12148, #3251 ) ) ;
#9212 = FACE_BOUND ( 'NONE', #10790, .T. ) ;
#9211 = AXIS2_PLACEMENT_3D ( 'NONE', #8337, #12776, #5101 ) ;
#9213 = VECTOR ( 'NONE', #5324, 1000.000000000000000 ) ;
#9214 = DIRECTION ( 'NONE',  ( 1.000000000000000000, 0.000000000000000000, 0.000000000000000000 ) ) ;
#9216 = VECTOR ( 'NONE', #13209, 1000.000000000000000 ) ;
#9215 = DIRECTION ( 'NONE',  ( 0.000000000000000000, 0.000000000000000000, -1.000000000000000000 ) ) ;
#9217 = VERTEX_POINT ( 'NONE', #10051 ) ;
#9218 = PLANE ( 'NONE',  #8278 ) ;
#9219 = LINE ( 'NONE', #4807, #8059 ) ;
#9220 = CARTESIAN_POINT ( 'NONE',  ( 0.000000000000000000, 0.000000000000000000, -5.000000000000000000 ) ) ;
#9221 = VECTOR ( 'NONE', #11358, 1000.000000000000000 ) ;
#9222 = DIRECTION ( 'NONE',  ( 0.8660254037844382635, 0.5000000000000004441, 0.000000000000000000 ) ) ;
#9223 = EDGE_LOOP ( 'NONE', ( #5435, #7815, #2112, #10647 ) ) ;
#9224 = AXIS2_PLACEMENT_3D ( 'NONE', #9941, #8681, #3914 ) ;
#9225 = CARTESIAN_POINT ( 'NONE',  ( 639.0000000000000000, 156.0000000000000000, -233.5000000000000000 ) ) ;
#9226 = DIRECTION ( 'NONE',  ( 0.000000000000000000, 0.000000000000000000, 1.000000000000000000 ) ) ;
#9227 = FACE_OUTER_BOUND ( 'NONE', #10545, .T. ) ;
#9228 = ITEM_DEFINED_TRANSFORMATION ( 'NONE', 'NONE', #1946,  #9440 ) ;
#9229 = ORIENTED_EDGE ( 'NONE', *, *, #3222, .F. ) ;
#9230 = VECTOR ( 'NONE', #6412, 1000.000000000000000 ) ;
#9231 = LINE ( 'NONE', #12547, #11564 ) ;
#9232 =( GEOMETRIC_REPRESENTATION_CONTEXT ( 3 ) GLOBAL_UNCERTAINTY_ASSIGNED_CONTEXT ( ( #4886 ) ) GLOBAL_UNIT_ASSIGNED_CONTEXT ( ( #12067, #775, #6316 ) ) REPRESENTATION_CONTEXT ( 'NONE', 'WORKASPACE' ) );
#9233 = ORIENTED_EDGE ( 'NONE', *, *, #11131, .T. ) ;
#9234 = ORIENTED_EDGE ( 'NONE', *, *, #5394, .F. ) ;
#9235 = DIRECTION ( 'NONE',  ( -1.000000000000000000, -0.000000000000000000, -0.000000000000000000 ) ) ;
#9236 = CARTESIAN_POINT ( 'NONE',  ( 0.000000000000000000, -3.464101615137750834, 2.000000000000007994 ) ) ;
#9237 = CARTESIAN_POINT ( 'NONE',  ( 2.682243648011666703, 3.070208061305304881, -0.04852650426601266831 ) ) ;
#9238 = AXIS2_PLACEMENT_3D ( 'NONE', #6093, #10595, #1451 ) ;
#9239 = ADVANCED_FACE ( 'NONE', ( #11309 ), #10349, .T. ) ;
#9240 = CARTESIAN_POINT ( 'NONE',  ( 0.03458865240849798295, 0.7871057074736624859, 3.999999999999995559 ) ) ;
#9241 = PRESENTATION_LAYER_ASSIGNMENT (  '', '', ( #11352 ) ) ;
#9242 = CARTESIAN_POINT ( 'NONE',  ( -6.815830331203685866, -1.210827632163352847E-13, -6.171384342982610960 ) ) ;
#9243 = ORIENTED_EDGE ( 'NONE', *, *, #4958, .T. ) ;
#9244 = DIRECTION ( 'NONE',  ( 1.000000000000000000, -0.000000000000000000, 0.000000000000000000 ) ) ;
#9245 = CARTESIAN_POINT ( 'NONE',  ( -1.312671235360383548, -3.860931062424228788, -0.05923475698271369466 ) ) ;
#9246 = VECTOR ( 'NONE', #7957, 1000.000000000000000 ) ;
#9247 = DIRECTION ( 'NONE',  ( 0.000000000000000000, 0.000000000000000000, 1.000000000000000000 ) ) ;
#9248 = ORIENTED_EDGE ( 'NONE', *, *, #10795, .F. ) ;
#9249 = ORIENTED_EDGE ( 'NONE', *, *, #13062, .T. ) ;
#9250 = CARTESIAN_POINT ( 'NONE',  ( 6.831985876597697072, -3.295913427296349951, -6.443925148804115821 ) ) ;
#9251 = FACE_OUTER_BOUND ( 'NONE', #505, .T. ) ;
#9252 = PRODUCT_DEFINITION_FORMATION_WITH_SPECIFIED_SOURCE ( 'ANY', '', #12393, .NOT_KNOWN. ) ;
#9253 = CARTESIAN_POINT ( 'NONE',  ( -5.979512004945809700, 4.053280633787070819, -0.5609245978742248839 ) ) ;
#9254 = EDGE_CURVE ( 'NONE', #6357, #8076, #3106, .T. ) ;
#9255 = VERTEX_POINT ( 'NONE', #10131 ) ;
#9256 = AXIS2_PLACEMENT_3D ( 'NONE', #8941, #1103, #12471 ) ;
#9257 = EDGE_LOOP ( 'NONE', ( #11233, #6433 ) ) ;
#9258 = CARTESIAN_POINT ( 'NONE',  ( 7.240873133980776366, 470.9098836221796773, 190.0000000000001990 ) ) ;
#9259 = CARTESIAN_POINT ( 'NONE',  ( 3.783380760145018981E-16, -7.895640089090872671, -6.564402953523720718 ) ) ;
#9260 = ADVANCED_FACE ( 'NONE', ( #9251 ), #4678, .T. ) ;
#9261 = DIRECTION ( 'NONE',  ( 0.000000000000000000, -1.000000000000000000, 0.000000000000000000 ) ) ;
#9262 = DIRECTION ( 'NONE',  ( 0.000000000000000000, 0.000000000000000000, 1.000000000000000000 ) ) ;
#9263 = CARTESIAN_POINT ( 'NONE',  ( -2.000000000000000000, -6.429618962271402616, -1.000000000000000000 ) ) ;
#9264 = CARTESIAN_POINT ( 'NONE',  ( -2.449848172108560540, -3.432307619358754724, -3.503702292528910078 ) ) ;
#9265 = SHAPE_REPRESENTATION_RELATIONSHIP ( 'NONE' , 'NONE' ,  #3392, #7736 ) ;
#9266 = ORIENTED_EDGE ( 'NONE', *, *, #222, .T. ) ;
#9267 = FACE_OUTER_BOUND ( 'NONE', #4716, .T. ) ;
#9268 = VERTEX_POINT ( 'NONE', #10279 ) ;
#9269 = VERTEX_POINT ( 'NONE', #9169 ) ;
#9270 = VECTOR ( 'NONE', #6897, 1000.000000000000000 ) ;
#9271 = CARTESIAN_POINT ( 'NONE',  ( 655.0000000000000000, 160.0000000000000284, 187.5000000000000000 ) ) ;
#9272 = VECTOR ( 'NONE', #8868, 1000.000000000000000 ) ;
#9273 = EDGE_CURVE ( 'NONE', #818, #3424, #9432, .T. ) ;
#9274 = CARTESIAN_POINT ( 'NONE',  ( 639.0000000000000000, 164.0000000000000000, -225.5000000000000000 ) ) ;
#9275 = DIRECTION ( 'NONE',  ( -1.000000000000000000, -0.000000000000000000, -0.000000000000000000 ) ) ;
#9276 = VERTEX_POINT ( 'NONE', #2454 ) ;
#9277 = PLANE ( 'NONE',  #4062 ) ;
#9278 = DIRECTION ( 'NONE',  ( 1.000000000000000000, 0.000000000000000000, 0.000000000000000000 ) ) ;
#9279 = EDGE_CURVE ( 'NONE', #8873, #9391, #6956, .T. ) ;
#9280 = CLOSED_SHELL ( 'NONE', ( #12383, #12488, #14150, #4027, #8724, #7014, #11718, #5931, #3865, #13585, #1598, #13795, #6444, #11546, #10040, #1687, #13936, #7264, #13727, #5502, #2681, #6386, #7108, #14319, #9239, #7107, #7607, #5649, #9692, #6501, #1462, #3044, #6822, #14592, #13058, #11621 ) ) ;
#9281 = DIRECTION ( 'NONE',  ( -1.000000000000000000, 0.000000000000000000, 0.000000000000000000 ) ) ;
#9282 = CARTESIAN_POINT ( 'NONE',  ( 1.655952806101427033, -3.662737355149048302, -1.182683869819604841E-14 ) ) ;
#9283 = ORIENTED_EDGE ( 'NONE', *, *, #4940, .T. ) ;
#9284 = EDGE_CURVE ( 'NONE', #13098, #5414, #1344, .T. ) ;
#9285 = CARTESIAN_POINT ( 'NONE',  ( 0.1586754815284889819, 4.240386000424035018, 0.6554360035617970981 ) ) ;
#9286 = ORIENTED_EDGE ( 'NONE', *, *, #9945, .T. ) ;
#9287 = ORIENTED_EDGE ( 'NONE', *, *, #9471, .T. ) ;
#9288 = CARTESIAN_POINT ( 'NONE',  ( 448.9584422793565750, 264.0194060144110608, 190.0000000000000000 ) ) ;
#9289 = CARTESIAN_POINT ( 'NONE',  ( -4.000000000000000000, -0.7890432684750890990, -0.04868663549882315533 ) ) ;
#9290 = CARTESIAN_POINT ( 'NONE',  ( 3.500000000000000000, -2.309401076758485161, 3.999999999999999112 ) ) ;
#9291 = ORIENTED_EDGE ( 'NONE', *, *, #3222, .T. ) ;
#9292 = DIRECTION ( 'NONE',  ( -0.000000000000000000, -0.000000000000000000, -1.000000000000000000 ) ) ;
#9293 = CARTESIAN_POINT ( 'NONE',  ( -6.500000000000000888, -2.534234941938113828, -0.3584823952106175882 ) ) ;
#9294 = DIRECTION ( 'NONE',  ( 0.03086419753086420623, 0.9995235871707959241, -0.000000000000000000 ) ) ;
#9295 = CARTESIAN_POINT ( 'NONE',  ( 1.390230914382191596, 4.043987460488659202, -3.502507215260488582 ) ) ;
#9296 = ORIENTED_EDGE ( 'NONE', *, *, #5824, .F. ) ;
#9297 = PRODUCT_DEFINITION ( 'UNKNOWN', '', #6661, #8708 ) ;
#9298 = CARTESIAN_POINT ( 'NONE',  ( 6.367873360227559232, -5.773502691896264416, 0.000000000000000000 ) ) ;
#9299 = SURFACE_SIDE_STYLE ('',( #339 ) ) ;
#9300 = ITEM_DEFINED_TRANSFORMATION ( 'NONE', 'NONE', #7131,  #9440 ) ;
#9301 = VERTEX_POINT ( 'NONE', #217 ) ;
#9302 = CARTESIAN_POINT ( 'NONE',  ( 639.0000000000000000, 156.0000000000000000, -225.5000000000000000 ) ) ;
#9303 = VERTEX_POINT ( 'NONE', #11523 ) ;
#9304 = EDGE_LOOP ( 'NONE', ( #7325, #1262, #4816, #11989 ) ) ;
#9305 = CARTESIAN_POINT ( 'NONE',  ( -9.999999999999957367, 376.8992337277236970, -187.0000000000000000 ) ) ;
#9306 = DIRECTION ( 'NONE',  ( 0.000000000000000000, 0.000000000000000000, -1.000000000000000000 ) ) ;
#9307 = EDGE_CURVE ( 'NONE', #8575, #12842, #10566, .T. ) ;
#9308 = DIRECTION ( 'NONE',  ( 0.000000000000000000, -1.000000000000000000, 0.000000000000000000 ) ) ;
#9309 = EDGE_CURVE ( 'NONE', #3851, #2440, #8128, .T. ) ;
#9310 = AXIS2_PLACEMENT_3D ( 'NONE', #5986, #2731, #7233 ) ;
#9311 = CARTESIAN_POINT ( 'NONE',  ( -4.517043073611196936E-16, 3.070647092368435693, 2.681483223904233437 ) ) ;
#9312 = UNCERTAINTY_MEASURE_WITH_UNIT (LENGTH_MEASURE( 1.000000000000000082E-05 ), #5222, 'distance_accuracy_value', 'NONE');
#9313 = CARTESIAN_POINT ( 'NONE',  ( 610.0000000000000000, 227.4403065089105951, 190.0000000000000000 ) ) ;
#9314 = ORIENTED_EDGE ( 'NONE', *, *, #769, .F. ) ;
#9315 = CARTESIAN_POINT ( 'NONE',  ( 635.0000000000000000, 160.0000000000000284, 210.0000000000000000 ) ) ;
#9316 = PLANE ( 'NONE',  #8202 ) ;
#9317 = CARTESIAN_POINT ( 'NONE',  ( 446.3084422793564841, 264.0194060144110608, 183.5000000000000000 ) ) ;
#9318 = DIRECTION ( 'NONE',  ( -1.000000000000000000, -0.000000000000000000, -0.000000000000000000 ) ) ;
#9319 = EDGE_CURVE ( 'NONE', #12461, #1135, #445, .T. ) ;
#9320 = ORIENTED_EDGE ( 'NONE', *, *, #14048, .F. ) ;
#9321 = ORIENTED_EDGE ( 'NONE', *, *, #347, .T. ) ;
#9322 = CARTESIAN_POINT ( 'NONE',  ( 638.7771423527817660, 153.4466020873429954, 210.0000119999999981 ) ) ;
#9323 = CARTESIAN_POINT ( 'NONE',  ( 629.0000000000000000, 154.0000000000000284, 187.5000000000000000 ) ) ;
#9324 = CARTESIAN_POINT ( 'NONE',  ( 6.245824673232988289, 3.903127342724162840, 3.450227696316072734 ) ) ;
#9325 = ORIENTED_EDGE ( 'NONE', *, *, #9885, .F. ) ;
#9326 = CIRCLE ( 'NONE', #4862, 4.250000000000000000 ) ;
#9327 = FACE_OUTER_BOUND ( 'NONE', #13594, .T. ) ;
#9328 = CARTESIAN_POINT ( 'NONE',  ( 6.527192678185238961, -2.941622124011228578, -5.095038975456188446 ) ) ;
#9329 = DIRECTION ( 'NONE',  ( -1.000000000000000000, 0.000000000000000000, -0.000000000000000000 ) ) ;
#9330 = CARTESIAN_POINT ( 'NONE',  ( 6.403457969954072126, 5.776886471390936251, -3.630823777237011237E-16 ) ) ;
#9331 = DIRECTION ( 'NONE',  ( 1.000000000000000000, 0.000000000000000000, 0.000000000000000000 ) ) ;
#9332 = CARTESIAN_POINT ( 'NONE',  ( 707.5067158355136598, 162.6912496279593938, -177.6000000000005059 ) ) ;
#9333 = APPLICATION_CONTEXT ( 'automotive_design' ) ;
#9334 = EDGE_CURVE ( 'NONE', #696, #3430, #7103, .T. ) ;
#9335 = VERTEX_POINT ( 'NONE', #4976 ) ;
#9336 = CARTESIAN_POINT ( 'NONE',  ( 2.725741868436127202, -3.045094352033990148, -3.220599429844051453 ) ) ;
#9337 = SHAPE_REPRESENTATION ( 'hex flange bolt small_iso_ISO 4162 - M8 x 35 x 22-N', ( #9440 ), #7588 ) ;
#9338 = ORIENTED_EDGE ( 'NONE', *, *, #1315, .T. ) ;
#9339 = ORIENTED_EDGE ( 'NONE', *, *, #6263, .T. ) ;
#9340 = CARTESIAN_POINT ( 'NONE',  ( 641.0000000000000000, 154.0000000000000568, -187.5000000000000000 ) ) ;
#9341 = CARTESIAN_POINT ( 'NONE',  ( 2.500000000000000000, -2.357898499370432166, 3.035766082959412415E-15 ) ) ;
#9342 = DIRECTION ( 'NONE',  ( 0.8191520442889923537, 0.000000000000000000, 0.5735764363510453823 ) ) ;
#9343 = DIRECTION ( 'NONE',  ( -0.9237280213470676626, -0.3830490080632388272, 0.000000000000000000 ) ) ;
#9344 = VERTEX_POINT ( 'NONE', #9323 ) ;
#9345 = CARTESIAN_POINT ( 'NONE',  ( -10.00000000000000888, 371.6790804732683569, 169.9999999999999716 ) ) ;
#9346 = DIRECTION ( 'NONE',  ( -1.000000000000000000, 0.000000000000000000, 0.000000000000000000 ) ) ;
#9347 = FACE_OUTER_BOUND ( 'NONE', #14540, .T. ) ;
#9348 = EDGE_CURVE ( 'NONE', #12661, #2075, #5112, .T. ) ;
#9349 = ORIENTED_EDGE ( 'NONE', *, *, #880, .F. ) ;
#9350 = SURFACE_STYLE_USAGE ( .BOTH. , #7276 ) ;
#9351 = VERTEX_POINT ( 'NONE', #6065 ) ;
#9352 = EDGE_CURVE ( 'NONE', #6863, #4259, #14111, .T. ) ;
#9353 = EDGE_LOOP ( 'NONE', ( #1886, #10669, #5756, #4230, #5503 ) ) ;
#9354 = DIRECTION ( 'NONE',  ( -1.000000000000000000, 0.000000000000000000, -0.000000000000000000 ) ) ;
#9355 = ADVANCED_FACE ( 'NONE', ( #13820 ), #10650, .F. ) ;
#9356 = ADVANCED_FACE ( 'NONE', ( #4830 ), #3717, .T. ) ;
#9357 = CYLINDRICAL_SURFACE ( 'NONE', #11772, 6.750000000000000000 ) ;
#9358 = DIRECTION ( 'NONE',  ( 0.000000000000000000, 0.000000000000000000, -1.000000000000000000 ) ) ;
#9359 = EDGE_CURVE ( 'NONE', #13232, #10717, #7177, .T. ) ;
#9360 = ORIENTED_EDGE ( 'NONE', *, *, #7087, .F. ) ;
#9361 = CARTESIAN_POINT ( 'NONE',  ( 609.9913795634330427, 185.6503456847118514, 184.8000000000000966 ) ) ;
#9362 = AXIS2_PLACEMENT_3D ( 'NONE', #4031, #7420, #8527 ) ;
#9363 = CARTESIAN_POINT ( 'NONE',  ( 152.8304684875957378, 364.5911659626319192, 210.0000000000000000 ) ) ;
#9364 = CARTESIAN_POINT ( 'NONE',  ( 6.500000000000000000, 3.752776749732573247, -0.8000000000000003775 ) ) ;
#9365 = CARTESIAN_POINT ( 'NONE',  ( -9.137956343300960071, 416.3137853645741302, 187.0000000000000000 ) ) ;
#9366 = ORIENTED_EDGE ( 'NONE', *, *, #11237, .T. ) ;
#9367 = CARTESIAN_POINT ( 'NONE',  ( 0.000000000000000000, 0.000000000000000000, 0.000000000000000000 ) ) ;
#9368 = ORIENTED_EDGE ( 'NONE', *, *, #8745, .F. ) ;
#9369 = CARTESIAN_POINT ( 'NONE',  ( -2.354826896168714434, -6.962563485461402024, 0.000000000000000000 ) ) ;
#9370 = ORIENTED_EDGE ( 'NONE', *, *, #8372, .F. ) ;
#9371 = ORIENTED_EDGE ( 'NONE', *, *, #847, .T. ) ;
#9372 =( NAMED_UNIT ( * ) SI_UNIT ( $, .STERADIAN. ) SOLID_ANGLE_UNIT ( ) );
#9373 = CARTESIAN_POINT ( 'NONE',  ( 0.000000000000000000, 0.000000000000000000, -4.974599999999998801 ) ) ;
#9374 = EDGE_CURVE ( 'NONE', #13232, #10137, #12710, .T. ) ;
#9375 = VECTOR ( 'NONE', #5004, 1000.000000000000000 ) ;
#9376 = EDGE_CURVE ( 'NONE', #11996, #3047, #6221, .T. ) ;
#9378 = CARTESIAN_POINT ( 'NONE',  ( 6.481779955677554383, -2.910222513313215131, 5.040653254389295235 ) ) ;
#9377 = AXIS2_PLACEMENT_3D ( 'NONE', #7187, #8137, #1435 ) ;
#9379 = AXIS2_PLACEMENT_3D ( 'NONE', #2592, #12999, #2669 ) ;
#9380 = LINE ( 'NONE', #13967, #14173 ) ;
#9381 = CARTESIAN_POINT ( 'NONE',  ( 628.0000000000000000, 152.9999999999999147, -233.5000000000000000 ) ) ;
#9382 = ORIENTED_EDGE ( 'NONE', *, *, #1952, .T. ) ;
#9383 = AXIS2_PLACEMENT_3D ( 'NONE', #3039, #12032, #7759 ) ;
#9384 = EDGE_CURVE ( 'NONE', #8013, #2514, #6634, .T. ) ;
#9385 = AXIS2_PLACEMENT_3D ( 'NONE', #7331, #10661, #9486 ) ;
#9386 = DIRECTION ( 'NONE',  ( 1.000000000000000000, 0.000000000000000000, 0.000000000000000000 ) ) ;
#9387 = CARTESIAN_POINT ( 'NONE',  ( 0.000000000000000000, 0.000000000000000000, 210.0000000000000000 ) ) ;
#9388 = DIRECTION ( 'NONE',  ( 1.000000000000000000, 0.000000000000000000, 0.000000000000000000 ) ) ;
#9389 = FACE_BOUND ( 'NONE', #4813, .T. ) ;
#9390 = ORIENTED_EDGE ( 'NONE', *, *, #3455, .T. ) ;
#9391 = VERTEX_POINT ( 'NONE', #11820 ) ;
#9392 = CARTESIAN_POINT ( 'NONE',  ( 642.5000000000001137, 160.0000000000000284, 210.0000059999999849 ) ) ;
#9393 = CARTESIAN_POINT ( 'NONE',  ( 631.0000000000000000, 155.9999999999999432, -225.5000000000000000 ) ) ;
#9394 = CARTESIAN_POINT ( 'NONE',  ( -3.811597179862308060, 5.304926841629211687, -0.01956314070068241109 ) ) ;
#9395 = CIRCLE ( 'NONE', #3029, 2.649999999999985700 ) ;
#9396 = AXIS2_PLACEMENT_3D ( 'NONE', #9468, #1411, #11593 ) ;
#9397 = CIRCLE ( 'NONE', #1840, 4.000000000000000000 ) ;
#9398 = ORIENTED_EDGE ( 'NONE', *, *, #14023, .T. ) ;
#9399 = DIRECTION ( 'NONE',  ( 1.000000000000000000, 0.000000000000000000, 0.000000000000000000 ) ) ;
#9400 = DIRECTION ( 'NONE',  ( 0.9578262852211513190, -0.2873478855663453846, 0.000000000000000000 ) ) ;
#9401 = DIRECTION ( 'NONE',  ( 0.000000000000000000, 0.000000000000000000, 1.000000000000000000 ) ) ;
#9402 = CARTESIAN_POINT ( 'NONE',  ( -10.00000000000000000, 413.4403065089105667, -190.0000000000000000 ) ) ;
#9403 = LINE ( 'NONE', #10362, #13849 ) ;
#9404 = CARTESIAN_POINT ( 'NONE',  ( -1.391697335622809950, -4.043246145443391448, -3.503898532754372575 ) ) ;
#9405 =( NAMED_UNIT ( * ) PLANE_ANGLE_UNIT ( ) SI_UNIT ( $, .RADIAN. ) );
#9406 = ORIENTED_EDGE ( 'NONE', *, *, #8352, .T. ) ;
#9407 = DIRECTION ( 'NONE',  ( 1.000000000000000000, 0.000000000000000000, 0.000000000000000000 ) ) ;
#9408 = CIRCLE ( 'NONE', #5629, 2.649999999999985700 ) ;
#9409 = ORIENTED_EDGE ( 'NONE', *, *, #2718, .T. ) ;
#9410 = ORIENTED_EDGE ( 'NONE', *, *, #12832, .T. ) ;
#9411 = CARTESIAN_POINT ( 'NONE',  ( 112.9652219749295341, 376.5507399164317803, -190.0000000000000000 ) ) ;
#9412 = CARTESIAN_POINT ( 'NONE',  ( 144.7991633467111683, 386.6211705227183870, 210.0000000000000000 ) ) ;
#9413 = EDGE_CURVE ( 'NONE', #11816, #12048, #8518, .T. ) ;
#9414 = CARTESIAN_POINT ( 'NONE',  ( 629.0000000000000000, 154.0000000000000284, 187.5000000000000000 ) ) ;
#9415 = CIRCLE ( 'NONE', #14368, 4.250000000000000000 ) ;
#9416 = DIRECTION ( 'NONE',  ( 9.963058866566173311E-16, 3.321019622188723911E-15, 1.000000000000000000 ) ) ;
#9417 = AXIS2_PLACEMENT_3D ( 'NONE', #1231, #2188, #3605 ) ;
#9418 = ORIENTED_EDGE ( 'NONE', *, *, #7212, .F. ) ;
#9419 = CARTESIAN_POINT ( 'NONE',  ( -8.542937654374687995, 1.046208125374536008E-15, -6.800000000000000711 ) ) ;
#9420 = CARTESIAN_POINT ( 'NONE',  ( -9.999999999999998224, 376.8992337277234128, 187.0000000000000000 ) ) ;
#9421 = FACE_OUTER_BOUND ( 'NONE', #10885, .T. ) ;
#9422 = DIRECTION ( 'NONE',  ( 0.000000000000000000, 0.000000000000000000, -1.000000000000000000 ) ) ;
#9423 = FILL_AREA_STYLE_COLOUR ( '', #9699 ) ;
#9424 = ORIENTED_EDGE ( 'NONE', *, *, #10156, .F. ) ;
#9425 = VECTOR ( 'NONE', #172, 1000.000000000000000 ) ;
#9426 = DIRECTION ( 'NONE',  ( 1.000000000000000000, 0.000000000000000000, 0.000000000000000000 ) ) ;
#9427 = ORIENTED_EDGE ( 'NONE', *, *, #4232, .T. ) ;
#9428 = CONICAL_SURFACE ( 'NONE', #3064, 6.500000000000000888, 0.8987552595851582282 ) ;
#9429 = AXIS2_PLACEMENT_3D ( 'NONE', #7184, #11674, #1503 ) ;
#9430 = CARTESIAN_POINT ( 'NONE',  ( 610.0000000000000000, 227.4403065089105951, -187.0000000000000000 ) ) ;
#9431 = CARTESIAN_POINT ( 'NONE',  ( 6.826399921716642005, 2.638123634694624631, -6.344399053232583796 ) ) ;
#9432 = CIRCLE ( 'NONE', #4480, 4.799999999999999822 ) ;
#9433 = EDGE_CURVE ( 'NONE', #1936, #2990, #2517, .T. ) ;
#9434 = AXIS2_PLACEMENT_3D ( 'NONE', #12355, #1290, #82 ) ;
#9435 = CARTESIAN_POINT ( 'NONE',  ( 635.0000000000000000, 160.0000000000000284, -222.5000000000000000 ) ) ;
#9436 = ORIENTED_EDGE ( 'NONE', *, *, #7979, .T. ) ;
#9437 = CARTESIAN_POINT ( 'NONE',  ( 609.6767525226840689, 186.8636552924789669, 187.9956429438695977 ) ) ;
#9438 = EDGE_CURVE ( 'NONE', #10367, #4352, #5203, .T. ) ;
#9439 = AXIS2_PLACEMENT_3D ( 'NONE', #9781, #6601, #11100 ) ;
#9440 = AXIS2_PLACEMENT_3D ( 'NONE', #4347, #14302, #6417 ) ;
#9441 = CARTESIAN_POINT ( 'NONE',  ( 610.4899793196105975, 188.8968529749589038, -185.7755421771552165 ) ) ;
#9442 = CARTESIAN_POINT ( 'NONE',  ( 610.8620436566991430, 188.5525593289318920, -184.8000000000000682 ) ) ;
#9443 = CARTESIAN_POINT ( 'NONE',  ( 0.04201760816084220557, -0.9730571234389052693, -5.000000000000000888 ) ) ;
#9444 = VERTEX_POINT ( 'NONE', #527 ) ;
#9445 = EDGE_CURVE ( 'NONE', #12510, #7620, #3081, .T. ) ;
#9446 = SURFACE_STYLE_USAGE ( .BOTH. , #10842 ) ;
#9447 = LINE ( 'NONE', #2720, #11253 ) ;
#9448 = ORIENTED_EDGE ( 'NONE', *, *, #14247, .T. ) ;
#9449 = AXIS2_PLACEMENT_3D ( 'NONE', #8859, #8929, #13651 ) ;
#9451 = ADVANCED_FACE ( 'NONE', ( #1633, #14047, #12929 ), #1718, .T. ) ;
#9450 = DIRECTION ( 'NONE',  ( 0.000000000000000000, 0.000000000000000000, 1.000000000000000000 ) ) ;
#9452 = ORIENTED_EDGE ( 'NONE', *, *, #2264, .F. ) ;
#9453 = ORIENTED_EDGE ( 'NONE', *, *, #9803, .T. ) ;
#9454 = DIRECTION ( 'NONE',  ( 0.000000000000000000, 0.000000000000000000, -1.000000000000000000 ) ) ;
#9455 =( GEOMETRIC_REPRESENTATION_CONTEXT ( 3 ) GLOBAL_UNCERTAINTY_ASSIGNED_CONTEXT ( ( #11224 ) ) GLOBAL_UNIT_ASSIGNED_CONTEXT ( ( #851, #5371, #12006 ) ) REPRESENTATION_CONTEXT ( 'NONE', 'WORKASPACE' ) );
#9456 = CARTESIAN_POINT ( 'NONE',  ( 6.500000000000000000, 3.752776749732563921, -8.000000000000000000 ) ) ;
#9457 = FACE_OUTER_BOUND ( 'NONE', #9500, .T. ) ;
#9458 = AXIS2_PLACEMENT_3D ( 'NONE', #963, #6583, #6514 ) ;
#9459 = DIRECTION ( 'NONE',  ( 0.000000000000000000, -1.000000000000000000, 0.000000000000000000 ) ) ;
#9460 = CIRCLE ( 'NONE', #12753, 6.500000000000000888 ) ;
#9461 = PRODUCT_DEFINITION_CONTEXT ( 'detailed design', #4066, 'design' ) ;
#9462 = DIRECTION ( 'NONE',  ( 0.000000000000000000, 0.000000000000000000, 1.000000000000000000 ) ) ;
#9463 = ORIENTED_EDGE ( 'NONE', *, *, #5983, .F. ) ;
#9464 = VECTOR ( 'NONE', #7805, 1000.000000000000114 ) ;
#9465 = EDGE_CURVE ( 'NONE', #8669, #2732, #8719, .T. ) ;
#9466 = COLOUR_RGB ( '',1.000000000000000000, 0.9490196078431372140, 0.9098039215686274384 ) ;
#9467 = CARTESIAN_POINT ( 'NONE',  ( 629.7500000000000000, 160.0000000000000284, -207.0000000000000000 ) ) ;
#9468 = CARTESIAN_POINT ( 'NONE',  ( 1.399999999999999689, 0.000000000000000000, -7.399999999999999467 ) ) ;
#9469 = DIRECTION ( 'NONE',  ( -0.9237280213470682178, -0.3830490080632377725, 0.000000000000000000 ) ) ;
#9471 = EDGE_CURVE ( 'NONE', #2514, #14470, #4088, .T. ) ;
#9470 = CARTESIAN_POINT ( 'NONE',  ( 710.3801946911771665, 172.2695124801717270, 9.266195726029882063E-13 ) ) ;
#9472 = ORIENTED_EDGE ( 'NONE', *, *, #1821, .F. ) ;
#9473 = VERTEX_POINT ( 'NONE', #1996 ) ;
#9474 = VECTOR ( 'NONE', #1898, 1000.000000000000114 ) ;
#9475 = CARTESIAN_POINT ( 'NONE',  ( 3.999999999999999112, -1.539600717839012978, -3.300726591567080703 ) ) ;
#9476 = CARTESIAN_POINT ( 'NONE',  ( 3.500000000000000000, 0.000000000000000000, 0.000000000000000000 ) ) ;
#9477 = AXIS2_PLACEMENT_3D ( 'NONE', #8064, #5626, #11387 ) ;
#9478 = FACE_OUTER_BOUND ( 'NONE', #2006, .T. ) ;
#9479 = MECHANICAL_DESIGN_GEOMETRIC_PRESENTATION_REPRESENTATION (  '', ( #14429 ), #3110 ) ;
#9480 = PLANE ( 'NONE',  #688 ) ;
#9481 = ORIENTED_EDGE ( 'NONE', *, *, #6365, .F. ) ;
#9482 = VECTOR ( 'NONE', #413, 1000.000000000000114 ) ;
#9483 = AXIS2_PLACEMENT_3D ( 'NONE', #11339, #3441, #9199 ) ;
#9484 = CARTESIAN_POINT ( 'NONE',  ( 103.3965373855728558, 344.6551246185656510, 190.0000000000000000 ) ) ;
#9485 = CARTESIAN_POINT ( 'NONE',  ( 6.452281807715712247, -2.898928808473065999, -5.021091983800445746 ) ) ;
#9486 = DIRECTION ( 'NONE',  ( -1.000000000000000000, 0.000000000000000000, 0.000000000000000000 ) ) ;
#9487 = LINE ( 'NONE', #8211, #10074 ) ;
#9488 = PRODUCT_DEFINITION_SHAPE ( 'NONE', 'NONE',  #14623 ) ;
#9489 = ORIENTED_EDGE ( 'NONE', *, *, #1499, .F. ) ;
#9490 = AXIS2_PLACEMENT_3D ( 'NONE', #10027, #7470, #8511 ) ;
#9491 = CARTESIAN_POINT ( 'NONE',  ( 125.3981793592638923, -37.61945380777919468, 182.7999999999996135 ) ) ;
#9492 = ORIENTED_EDGE ( 'NONE', *, *, #664, .F. ) ;
#9493 = ORIENTED_EDGE ( 'NONE', *, *, #3711, .T. ) ;
#9494 = DIRECTION ( 'NONE',  ( 1.000000000000000000, 0.000000000000000000, 0.000000000000000000 ) ) ;
#9495 = AXIS2_PLACEMENT_3D ( 'NONE', #7151, #5024, #9519 ) ;
#9496 = LINE ( 'NONE', #1661, #2599 ) ;
#9497 = DIRECTION ( 'NONE',  ( -0.000000000000000000, -0.000000000000000000, -1.000000000000000000 ) ) ;
#9498 = ADVANCED_FACE ( 'NONE', ( #2060 ), #811, .F. ) ;
#9499 = DIRECTION ( 'NONE',  ( 1.000000000000000000, -0.000000000000000000, 0.000000000000000000 ) ) ;
#9500 = EDGE_LOOP ( 'NONE', ( #10492, #5163, #9678, #1062 ) ) ;
#9501 = DIRECTION ( 'NONE',  ( 2.312964634635740689E-15, -1.000000000000000000, 0.000000000000000000 ) ) ;
#9502 = CARTESIAN_POINT ( 'NONE',  ( 707.5067158355134325, 162.6912496279593086, -182.7999999999999261 ) ) ;
#9503 = DIRECTION ( 'NONE',  ( 0.000000000000000000, 0.000000000000000000, -1.000000000000000000 ) ) ;
#9504=STYLED_ITEM('',(#14660),#11971);
#9505 = ORIENTED_EDGE ( 'NONE', *, *, #14037, .T. ) ;
#9506 = CIRCLE ( 'NONE', #3142, 5.000000000000004441 ) ;
#9507 = DIRECTION ( 'NONE',  ( -0.9578262852211506528, 0.2873478855663477161, -0.000000000000000000 ) ) ;
#9508 = CARTESIAN_POINT ( 'NONE',  ( 0.000000000000000000, 0.000000000000000000, -7.381345277524544279 ) ) ;
#9509 = VERTEX_POINT ( 'NONE', #14263 ) ;
#9510 = EDGE_CURVE ( 'NONE', #1371, #10838, #2114, .T. ) ;
#9511 = VECTOR ( 'NONE', #11839, 1000.000000000000000 ) ;
#9512 = EDGE_CURVE ( 'NONE', #12112, #6053, #3120, .T. ) ;
#9513 = CARTESIAN_POINT ( 'NONE',  ( 4.211140560182196957, 2.431303136016536470, -3.745885042887433514 ) ) ;
#9514 = LINE ( 'NONE', #7501, #13424 ) ;
#9515 = FACE_OUTER_BOUND ( 'NONE', #3967, .T. ) ;
#9516 = CLOSED_SHELL ( 'NONE', ( #13455, #7832, #6922, #5013, #9739, #14236, #11333, #11945, #10177, #9260, #3962, #7785, #13065, #2528, #7529, #6548, #4290, #5225, #7384, #13502, #6045, #4157, #11978, #7650, #4084, #11230, #1235, #14233 ) ) ;
#9517 = VERTEX_POINT ( 'NONE', #1777 ) ;
#9518 = FACE_OUTER_BOUND ( 'NONE', #8821, .T. ) ;
#9519 = DIRECTION ( 'NONE',  ( 0.000000000000000000, 0.000000000000000000, -1.000000000000000000 ) ) ;
#9520 = CARTESIAN_POINT ( 'NONE',  ( 0.000000000000000000, 0.000000000000000000, -1.000000000000000000 ) ) ;
#9521 = CARTESIAN_POINT ( 'NONE',  ( 0.000000000000000000, 0.000000000000000000, -5.000000000000000000 ) ) ;
#9522 = EDGE_LOOP ( 'NONE', ( #3267, #10383, #11664, #11260 ) ) ;
#9523 = PRESENTATION_STYLE_ASSIGNMENT (( #5028 ) ) ;
#9524 = PRESENTATION_STYLE_ASSIGNMENT (( #10542 ) ) ;
#9525 = ORIENTED_EDGE ( 'NONE', *, *, #240, .T. ) ;
#9526 = ORIENTED_EDGE ( 'NONE', *, *, #7699, .T. ) ;
#9527 = EDGE_CURVE ( 'NONE', #5202, #6863, #5328, .T. ) ;
#9528 = LINE ( 'NONE', #10327, #11806 ) ;
#9529 = B_SPLINE_CURVE_WITH_KNOTS ( 'NONE', 3,
 ( #8469, #11786, #12834, #4873, #11707, #10693, #2715, #5025, #4061, #9364 ),
 .UNSPECIFIED., .F., .F.,
 ( 4, 2, 2, 2, 4 ),
 ( 0.009353627468483380336, 0.01031000219096067476, 0.01126637691343796918, 0.01222275163591526534, 0.01317912635839255976 ),
 .UNSPECIFIED. ) ;
#9530 = VERTEX_POINT ( 'NONE', #5478 ) ;
#9531 = CARTESIAN_POINT ( 'NONE',  ( 0.000000000000000000, 0.5192545390863916310, -1.000000000000000000 ) ) ;
#9532 = LINE ( 'NONE', #4202, #4006 ) ;
#9533 = CARTESIAN_POINT ( 'NONE',  ( 455.5035746174796714, 294.6698471414878782, -210.0000000000000000 ) ) ;
#9534 = LINE ( 'NONE', #3921, #11562 ) ;
#9535 = DIRECTION ( 'NONE',  ( 0.9578262852211513190, -0.2873478855663453846, -0.000000000000000000 ) ) ;
#9536 = ORIENTED_EDGE ( 'NONE', *, *, #4371, .T. ) ;
#9537 = DIRECTION ( 'NONE',  ( -1.000000000000000000, -0.000000000000000000, -0.000000000000000000 ) ) ;
#9538 = CARTESIAN_POINT ( 'NONE',  ( 2.999999999999999112, 2.309401076758500704, -4.000000000000000000 ) ) ;
#9539 = APPLICATION_PROTOCOL_DEFINITION ( 'draft international standard', 'automotive_design', 1998, #2821 ) ;
#9540 = ADVANCED_FACE ( 'NONE', ( #9827 ), #10783, .T. ) ;
#9541 = CARTESIAN_POINT ( 'NONE',  ( 0.000000000000000000, 0.000000000000000000, 0.000000000000000000 ) ) ;
#9542 = VERTEX_POINT ( 'NONE', #4004 ) ;
#9543 = VERTEX_POINT ( 'NONE', #11074 ) ;
#9544 = DIRECTION ( 'NONE',  ( 1.000000000000000000, 0.000000000000000000, 0.000000000000000000 ) ) ;
#9545 = DIRECTION ( 'NONE',  ( -1.000000000000000000, -0.000000000000000000, 0.000000000000000000 ) ) ;
#9546 = CARTESIAN_POINT ( 'NONE',  ( 0.2499999999999966416, -8.096141056083448362, -1.000000000000000000 ) ) ;
#9547 = EDGE_CURVE ( 'NONE', #5965, #6145, #13677, .T. ) ;
#9548 = EDGE_CURVE ( 'NONE', #14559, #4861, #7402, .T. ) ;
#9549 = DIRECTION ( 'NONE',  ( -1.000000000000000000, 0.000000000000000000, 0.000000000000000000 ) ) ;
#9550 = ORIENTED_EDGE ( 'NONE', *, *, #12406, .F. ) ;
#9551 = EDGE_CURVE ( 'NONE', #5571, #11290, #11550, .T. ) ;
#9552 = FACE_BOUND ( 'NONE', #6184, .T. ) ;
#9553 = CARTESIAN_POINT ( 'NONE',  ( 6.385552186430389021, -2.886751345948134873, -5.000000000000000000 ) ) ;
#9554 = CARTESIAN_POINT ( 'NONE',  ( 237.7887055630607733, 337.0156335382104089, 182.7999999999996135 ) ) ;
#9555 = PLANE ( 'NONE',  #1367 ) ;
#9556 = CARTESIAN_POINT ( 'NONE',  ( 164.3243839102495656, 402.9042173714779551, 210.0000000000000000 ) ) ;
#9557 = CARTESIAN_POINT ( 'NONE',  ( -6.270061300899934409, 4.268872906156499170, -6.443866470201760954 ) ) ;
#9558 = SURFACE_STYLE_FILL_AREA ( #7189 ) ;
#9559 = EDGE_LOOP ( 'NONE', ( #9789, #9418, #11791, #11391, #8451, #5244, #9360, #2082 ) ) ;
#9560 = LINE ( 'NONE', #10733, #7781 ) ;
#9561 = EDGE_LOOP ( 'NONE', ( #1940, #2220, #8507, #5700 ) ) ;
#9562 = ORIENTED_EDGE ( 'NONE', *, *, #7056, .T. ) ;
#9563 = LINE ( 'NONE', #606, #3096 ) ;
#9564 = EDGE_CURVE ( 'NONE', #14011, #7999, #4222, .T. ) ;
#9565 = FACE_OUTER_BOUND ( 'NONE', #5074, .T. ) ;
#9566 = CARTESIAN_POINT ( 'NONE',  ( 229.2257385731833779, 308.4724102386176128, -177.6000000000002217 ) ) ;
#9567 = DIRECTION ( 'NONE',  ( -1.000000000000000000, 0.000000000000000000, 0.000000000000000000 ) ) ;
#9568 = ORIENTED_EDGE ( 'NONE', *, *, #6073, .F. ) ;
#9569 = CARTESIAN_POINT ( 'NONE',  ( 107.2182642636026202, 357.3942142120087055, 210.0000000000000000 ) ) ;
#9570 = FACE_OUTER_BOUND ( 'NONE', #1475, .T. ) ;
#9571 = CARTESIAN_POINT ( 'NONE',  ( -3.472371940586054251, -2.614027278893156669, -3.320322319202162031 ) ) ;
#9572 = CYLINDRICAL_SURFACE ( 'NONE', #13269, 2.500000000000000444 ) ;
#9573 = VERTEX_POINT ( 'NONE', #879 ) ;
#9574 = EDGE_CURVE ( 'NONE', #151, #931, #3423, .T. ) ;
#9575 = CARTESIAN_POINT ( 'NONE',  ( 1.860380241283018377, 6.431462466365323927, -0.1499059597315287040 ) ) ;
#9576 = CARTESIAN_POINT ( 'NONE',  ( 6.367873360227556567, 2.886751345948122882, -5.000000000000000000 ) ) ;
#9577 = ORIENTED_EDGE ( 'NONE', *, *, #1124, .F. ) ;
#9578 = ADVANCED_FACE ( 'NONE', ( #10998 ), #7461, .T. ) ;
#9579 = CARTESIAN_POINT ( 'NONE',  ( 0.000000000000000000, 0.000000000000000000, 0.000000000000000000 ) ) ;
#9580 = CARTESIAN_POINT ( 'NONE',  ( -6.746558653881629120, 3.895127454924392385, -6.526045885145571823 ) ) ;
#9581 = CARTESIAN_POINT ( 'NONE',  ( 629.7500000000000000, 160.0000000000000284, 207.0000000000000000 ) ) ;
#9582 = VERTEX_POINT ( 'NONE', #1848 ) ;
#9583 = CARTESIAN_POINT ( 'NONE',  ( 610.3661002516460030, 189.1614810556852717, 186.1520027839448232 ) ) ;
#9584 = CARTESIAN_POINT ( 'NONE',  ( 610.7405786874708156, 188.6041887390371130, -185.0905558487023370 ) ) ;
#9585 = DIRECTION ( 'NONE',  ( 1.000000000000000000, 0.000000000000000000, 1.148424442117023040E-15 ) ) ;
#9586 = FACE_OUTER_BOUND ( 'NONE', #8218, .T. ) ;
#9587 = EDGE_LOOP ( 'NONE', ( #14541, #8814, #14076, #3850 ) ) ;
#9588 = DIRECTION ( 'NONE',  ( -8.745957808406929547E-15, -2.915319269468972624E-14, -1.000000000000000000 ) ) ;
#9589 = ORIENTED_EDGE ( 'NONE', *, *, #12069, .T. ) ;
#9590 = ORIENTED_EDGE ( 'NONE', *, *, #5893, .T. ) ;
#9591 = DIRECTION ( 'NONE',  ( 0.000000000000000000, 0.000000000000000000, 1.000000000000000000 ) ) ;
#9592 = FACE_OUTER_BOUND ( 'NONE', #5648, .T. ) ;
#9593 = FACE_OUTER_BOUND ( 'NONE', #7871, .T. ) ;
#9594 = PRODUCT_DEFINITION_SHAPE ( 'NONE', 'NONE',  #14629 ) ;
#9595 = EDGE_CURVE ( 'NONE', #7620, #12510, #7306, .T. ) ;
#9596 = DIRECTION ( 'NONE',  ( 0.000000000000000000, 0.000000000000000000, -1.000000000000000000 ) ) ;
#9597 = PRODUCT_DEFINITION_CONTEXT ( 'detailed design', #8854, 'design' ) ;
#9598 = LINE ( 'NONE', #11722, #7678 ) ;
#9599 = VERTEX_POINT ( 'NONE', #9765 ) ;
#9600 = PLANE ( 'NONE',  #10570 ) ;
#9601 = LINE ( 'NONE', #804, #2562 ) ;
#9602 =( NAMED_UNIT ( * ) SI_UNIT ( $, .STERADIAN. ) SOLID_ANGLE_UNIT ( ) );
#9603 = AXIS2_PLACEMENT_3D ( 'NONE', #112, #11366, #8927 ) ;
#9604 = DIRECTION ( 'NONE',  ( 0.000000000000000000, -1.000000000000000000, 0.000000000000000000 ) ) ;
#9605 = CONICAL_SURFACE ( 'NONE', #6543, 6.500000000000000888, 0.8987552595851582282 ) ;
#9606 = ORIENTED_EDGE ( 'NONE', *, *, #12686, .T. ) ;
#9607 = ORIENTED_EDGE ( 'NONE', *, *, #13158, .T. ) ;
#9608 = DIRECTION ( 'NONE',  ( -1.000000000000000000, 1.224646799147352714E-16, 0.000000000000000000 ) ) ;
#9609 = CARTESIAN_POINT ( 'NONE',  ( 8.500000000000000000, -2.886751345948134873, -5.000000000000000000 ) ) ;
#9610 = LINE ( 'NONE', #1778, #11511 ) ;
#9611 = APPLICATION_CONTEXT ( 'automotive_design' ) ;
#9612 = EDGE_CURVE ( 'NONE', #1794, #3289, #8645, .T. ) ;
#9613 = CARTESIAN_POINT ( 'NONE',  ( 0.000000000000000000, 0.000000000000000000, -233.5000000000000000 ) ) ;
#9615 = ORIENTED_EDGE ( 'NONE', *, *, #6914, .T. ) ;
#9614 = VECTOR ( 'NONE', #3119, 999.9999999999998863 ) ;
#9616 = VECTOR ( 'NONE', #10143, 1000.000000000000114 ) ;
#9617 = DIRECTION ( 'NONE',  ( 1.921916333308134107E-15, 6.406387777693825847E-15, -1.000000000000000000 ) ) ;
#9618 = CARTESIAN_POINT ( 'NONE',  ( 6.781345014477444977, 3.590342129888852263, -6.122077150241850951 ) ) ;
#9619 = CARTESIAN_POINT ( 'NONE',  ( 0.000000000000000000, 0.000000000000000000, 0.000000000000000000 ) ) ;
#9620 = EDGE_CURVE ( 'NONE', #10129, #3017, #12246, .T. ) ;
#9621 = LINE ( 'NONE', #11676, #14336 ) ;
#9622 = CARTESIAN_POINT ( 'NONE',  ( 1.411581201560190495E-15, 4.862606272033091592, -3.745885042887436622 ) ) ;
#9623 = CARTESIAN_POINT ( 'NONE',  ( -8.505790995055050985, 376.6597771564184995, -184.8000000000000398 ) ) ;
#9624 = FILL_AREA_STYLE_COLOUR ( '', #259 ) ;
#9625 = ORIENTED_EDGE ( 'NONE', *, *, #2560, .T. ) ;
#9626 = EDGE_CURVE ( 'NONE', #2500, #6946, #13655, .T. ) ;
#9627 = CARTESIAN_POINT ( 'NONE',  ( -2.000000000000002665, -3.464101615137770374, -3.142992957459237680 ) ) ;
#9628 = ORIENTED_EDGE ( 'NONE', *, *, #4639, .T. ) ;
#9629 = ORIENTED_EDGE ( 'NONE', *, *, #2151, .T. ) ;
#9630 = LINE ( 'NONE', #8522, #12513 ) ;
#9631 = VECTOR ( 'NONE', #10094, 1000.000000000000114 ) ;
#9632 = EDGE_CURVE ( 'NONE', #2694, #5396, #11437, .T. ) ;
#9633 = VECTOR ( 'NONE', #6455, 1000.000000000000000 ) ;
#9634 = CARTESIAN_POINT ( 'NONE',  ( 3.700000000000000178, 0.000000000000000000, 0.000000000000000000 ) ) ;
#9635 = FACE_OUTER_BOUND ( 'NONE', #9210, .T. ) ;
#9636 = PLANE ( 'NONE',  #1829 ) ;
#9637 = ORIENTED_EDGE ( 'NONE', *, *, #8467, .T. ) ;
#9638 = FACE_BOUND ( 'NONE', #6515, .T. ) ;
#9639 = CARTESIAN_POINT ( 'NONE',  ( 152.8304684875957378, 364.5911659626319192, -210.0000000000000000 ) ) ;
#9640 = VECTOR ( 'NONE', #12790, 1000.000000000000000 ) ;
#9641 = VECTOR ( 'NONE', #9986, 1000.000000000000000 ) ;
#9642 = PLANE ( 'NONE',  #7731 ) ;
#9643 = LINE ( 'NONE', #6180, #13501 ) ;
#9644 =( LENGTH_UNIT ( ) NAMED_UNIT ( * ) SI_UNIT ( .MILLI., .METRE. ) );
#9645 = ORIENTED_EDGE ( 'NONE', *, *, #7954, .F. ) ;
#9646 = EDGE_CURVE ( 'NONE', #11111, #12984, #2520, .T. ) ;
#9647 = EDGE_CURVE ( 'NONE', #12192, #2358, #4255, .T. ) ;
#9648 = FACE_OUTER_BOUND ( 'NONE', #2308, .T. ) ;
#9649 = CARTESIAN_POINT ( 'NONE',  ( 443.6584422793565636, 264.0194060144110608, 210.0000000000000000 ) ) ;
#9650 = CONTEXT_DEPENDENT_SHAPE_REPRESENTATION ( #551, #9488 ) ;
#9651 = ORIENTED_EDGE ( 'NONE', *, *, #130, .T. ) ;
#9652 = ADVANCED_FACE ( 'NONE', ( #10038 ), #2276, .F. ) ;
#9653 = CARTESIAN_POINT ( 'NONE',  ( -20.63749999999999929, 0.000000000000000000, -5.750000000000000000 ) ) ;
#9654 = CIRCLE ( 'NONE', #11749, 4.000000000000000000 ) ;
#9655 = AXIS2_PLACEMENT_3D ( 'NONE', #9613, #3802, #2908 ) ;
#9656 = DIRECTION ( 'NONE',  ( 0.000000000000000000, 0.000000000000000000, -1.000000000000000000 ) ) ;
#9657 = DIRECTION ( 'NONE',  ( -0.9914448613738102711, -0.1305261922200524338, 0.000000000000000000 ) ) ;
#9658 = EDGE_LOOP ( 'NONE', ( #9716, #6693, #5945, #5376 ) ) ;
#9659 = CARTESIAN_POINT ( 'NONE',  ( 610.7375075899259400, 188.5899201489639267, 185.0880224589102454 ) ) ;
#9660 = DIRECTION ( 'NONE',  ( -1.000000000000000000, 1.224646799147354686E-16, 0.000000000000000000 ) ) ;
#9661 = AXIS2_PLACEMENT_3D ( 'NONE', #1372, #11268, #5877 ) ;
#9662 = CARTESIAN_POINT ( 'NONE',  ( 635.0000000000000000, 160.0000000000000284, -217.5000000000000284 ) ) ;
#9663 = LINE ( 'NONE', #10620, #715 ) ;
#9664 = CARTESIAN_POINT ( 'NONE',  ( 627.5000000000000000, 160.0000000000000284, 210.0000119999999981 ) ) ;
#9665 = EDGE_LOOP ( 'NONE', ( #1922, #10018 ) ) ;
#9666 = AXIS2_PLACEMENT_3D ( 'NONE', #6046, #7008, #8335 ) ;
#9667 = TOROIDAL_SURFACE ( 'NONE', #6121, 7.399999999999999467, 0.1000000000000000472 ) ;
#9668 =( LENGTH_UNIT ( ) NAMED_UNIT ( * ) SI_UNIT ( .MILLI., .METRE. ) );
#9669 = ORIENTED_EDGE ( 'NONE', *, *, #1760, .T. ) ;
#9670 = ORIENTED_EDGE ( 'NONE', *, *, #4729, .F. ) ;
#9671 = PLANE ( 'NONE',  #7272 ) ;
#9672 = AXIS2_PLACEMENT_3D ( 'NONE', #12120, #6593, #13164 ) ;
#9673 = CARTESIAN_POINT ( 'NONE',  ( -4.000000000000000000, 2.309401076758498483, -3.433295621305379353 ) ) ;
#9674 = LINE ( 'NONE', #12016, #951 ) ;
#9675 = CARTESIAN_POINT ( 'NONE',  ( 10.00000000000000000, 10.00000000000000178, 210.0000000000000000 ) ) ;
#9676 = VECTOR ( 'NONE', #11889, 1000.000000000000000 ) ;
#9677 = CARTESIAN_POINT ( 'NONE',  ( -1.500000000000001332, 9.123618653647779187E-16, 7.399999999999999467 ) ) ;
#9678 = ORIENTED_EDGE ( 'NONE', *, *, #1428, .F. ) ;
#9679 = AXIS2_PLACEMENT_3D ( 'NONE', #10993, #3115, #6438 ) ;
#9680 = DIRECTION ( 'NONE',  ( -0.000000000000000000, -0.000000000000000000, -1.000000000000000000 ) ) ;
#9681 = CARTESIAN_POINT ( 'NONE',  ( -112.9080459801079144, 33.87241379403258890, -190.0000000000000000 ) ) ;
#9682 = APPLICATION_PROTOCOL_DEFINITION ( 'draft international standard', 'automotive_design', 1998, #1022 ) ;
#9683 = CIRCLE ( 'NONE', #11783, 0.7500000000000000000 ) ;
#9684 = DIRECTION ( 'NONE',  ( -0.2873478855663502141, -0.9578262852211498757, 3.895519384649669193E-15 ) ) ;
#9685 = VECTOR ( 'NONE', #5191, 1000.000000000000000 ) ;
#9686 =( BOUNDED_SURFACE ( )  B_SPLINE_SURFACE ( 3, 2, ( 
 ( #5820, #8254, #13804 ),
 ( #5902, #195, #8112 ),
 ( #5978, #341, #13737 ),
 ( #8175, #2659, #2577 ),
 ( #7079, #4952, #11580 ),
 ( #11433, #2499, #7001 ) ),
 .UNSPECIFIED., .F., .F., .T. ) 
 B_SPLINE_SURFACE_WITH_KNOTS ( ( 4, 2, 4 ),
 ( 3, 3 ),
 ( 0.02367497856332483747, 0.02662799652435013376, 0.02958101448537543005 ),
 ( 0.000000000000000000, 1.000000000000000000 ),
 .UNSPECIFIED. ) 
 GEOMETRIC_REPRESENTATION_ITEM ( )  RATIONAL_B_SPLINE_SURFACE ( (
 ( 1.000000000000000000, 0.8047781226141854649, 1.000000000000000000),
 ( 1.000000000000000000, 0.8123782257049820821, 1.000000000000000000),
 ( 1.000000000000000000, 0.8190665358012705344, 1.000000000000000000),
 ( 1.000000000000000000, 0.8192358187342196896, 1.000000000000000000),
 ( 1.000000000000000000, 0.8126132506074239537, 1.000000000000000000),
 ( 1.000000000000000000, 0.8047712440299316095, 1.000000000000000000) ) ) 
 REPRESENTATION_ITEM ( '' )  SURFACE ( )  );
#9687 = ORIENTED_EDGE ( 'NONE', *, *, #7396, .F. ) ;
#9688 = ORIENTED_EDGE ( 'NONE', *, *, #6837, .F. ) ;
#9689 = CARTESIAN_POINT ( 'NONE',  ( -5.384454397937118664, 6.594054843588581554E-16, -4.484454397937119197 ) ) ;
#9690 = DIRECTION ( 'NONE',  ( -0.000000000000000000, -0.000000000000000000, -1.000000000000000000 ) ) ;
#9691 = EDGE_CURVE ( 'NONE', #11174, #8728, #2354, .T. ) ;
#9692 = ADVANCED_FACE ( 'NONE', ( #12464 ), #5762, .F. ) ;
#9693 = CARTESIAN_POINT ( 'NONE',  ( -9.999999999999790390, 413.4403065089115330, -184.7999999999999829 ) ) ;
#9694 = AXIS2_PLACEMENT_3D ( 'NONE', #7973, #2366, #6874 ) ;
#9695 = CIRCLE ( 'NONE', #2623, 0.2000000000000000944 ) ;
#9696 = FACE_BOUND ( 'NONE', #4799, .T. ) ;
#9697 = AXIS2_PLACEMENT_3D ( 'NONE', #9533, #1916, #1987 ) ;
#9698 = ORIENTED_EDGE ( 'NONE', *, *, #8828, .T. ) ;
#9699 = COLOUR_RGB ( '',0.8941176470588234615, 0.8941176470588234615, 0.8941176470588234615 ) ;
#9700 = DIRECTION ( 'NONE',  ( -0.9237280213470682178, -0.3830490080632377725, 0.000000000000000000 ) ) ;
#9701 = CARTESIAN_POINT ( 'NONE',  ( 4.574783636564339950, 5.228990388887490681, -6.171384342982508819 ) ) ;
#9702 = CARTESIAN_POINT ( 'NONE',  ( 635.0000000000000000, 160.0000000000000284, 211.0000000000000000 ) ) ;
#9703 = ORIENTED_EDGE ( 'NONE', *, *, #9945, .F. ) ;
#9704 = PLANE ( 'NONE',  #7967 ) ;
#9705 = CARTESIAN_POINT ( 'NONE',  ( -4.211140560182196957, -2.431303136016552013, -3.745885042887436178 ) ) ;
#9706 = LINE ( 'NONE', #1791, #11040 ) ;
#9707 = CONICAL_SURFACE ( 'NONE', #3341, 6.500000000000000888, 0.8987552595851582282 ) ;
#9708 = EDGE_LOOP ( 'NONE', ( #7919, #11455, #2098, #10989, #8841, #7160, #10665, #13449, #1205, #13713, #6615, #10290, #11599, #6224, #14394, #8187, #10168, #12540, #750, #3076 ) ) ;
#9709 = VECTOR ( 'NONE', #8663, 1000.000000000000000 ) ;
#9710 = VERTEX_POINT ( 'NONE', #11152 ) ;
#9711 = EDGE_LOOP ( 'NONE', ( #2655, #13860, #13498 ) ) ;
#9712 = DIRECTION ( 'NONE',  ( 1.000000000000000000, 0.000000000000000000, 0.000000000000000000 ) ) ;
#9713 = EDGE_CURVE ( 'NONE', #13126, #2860, #391, .T. ) ;
#9714 = CARTESIAN_POINT ( 'NONE',  ( 237.7887055630607733, 337.0156335382104658, 182.7999999999996135 ) ) ;
#9715 = VECTOR ( 'NONE', #1666, 1000.000000000000114 ) ;
#9717 = EDGE_CURVE ( 'NONE', #9543, #344, #1656, .T. ) ;
#9716 = ORIENTED_EDGE ( 'NONE', *, *, #4595, .F. ) ;
#9718 = VERTEX_POINT ( 'NONE', #10113 ) ;
#9719 = DIRECTION ( 'NONE',  ( 0.000000000000000000, 0.000000000000000000, 1.000000000000000000 ) ) ;
#9720 = CARTESIAN_POINT ( 'NONE',  ( 630.3908996001882770, 165.9975013179864618, 210.0000119999999981 ) ) ;
#9721 = CARTESIAN_POINT ( 'NONE',  ( 443.6584422793565636, 264.0194060144110608, -190.0000000000000000 ) ) ;
#9722 = DIRECTION ( 'NONE',  ( 1.000000000000000000, 0.000000000000000000, 0.000000000000000000 ) ) ;
#9723 = VERTEX_POINT ( 'NONE', #3472 ) ;
#9724 = CARTESIAN_POINT ( 'NONE',  ( 455.5035746174796714, 294.6698471414878782, 190.0000000000000568 ) ) ;
#9725 = EDGE_LOOP ( 'NONE', ( #9044, #5575, #14219, #8111 ) ) ;
#9726 = CIRCLE ( 'NONE', #751, 2.499999999999999556 ) ;
#9727 = ADVANCED_FACE ( 'NONE', ( #14543 ), #11293, .F. ) ;
#9728 = ORIENTED_EDGE ( 'NONE', *, *, #5928, .F. ) ;
#9729 = PRODUCT_DEFINITION_SHAPE ( 'NONE', 'NONE',  #14637 ) ;
#9730 = AXIS2_PLACEMENT_3D ( 'NONE', #3864, #8344, #520 ) ;
#9731 = CARTESIAN_POINT ( 'NONE',  ( 3.500000000000000000, 3.306546357697854226E-16, 2.700000000000000622 ) ) ;
#9732 = EDGE_CURVE ( 'NONE', #9718, #2950, #7970, .T. ) ;
#9733 = PLANE ( 'NONE',  #4766 ) ;
#9734 = ADVANCED_FACE ( 'NONE', ( #1265 ), #10264, .F. ) ;
#9735 = COLOUR_RGB ( '',0.8941176470588234615, 0.8941176470588234615, 0.8941176470588234615 ) ;
#9736 = ORIENTED_EDGE ( 'NONE', *, *, #4446, .T. ) ;
#9737 = CARTESIAN_POINT ( 'NONE',  ( 3.680118525130245732, -2.494084732383344605, -0.3507732604232533524 ) ) ;
#9738 = DIRECTION ( 'NONE',  ( -0.8191520442889917986, 0.000000000000000000, -0.5735764363510460484 ) ) ;
#9739 = ADVANCED_FACE ( 'NONE', ( #6721 ), #14479, .F. ) ;
#9740 = PRODUCT_DEFINITION ( 'UNKNOWN', '', #1476, #13744 ) ;
#9741 = CARTESIAN_POINT ( 'NONE',  ( 0.000000000000000000, 0.000000000000000000, 0.000000000000000000 ) ) ;
#9742 = ORIENTED_EDGE ( 'NONE', *, *, #9626, .T. ) ;
#9743 = PLANE ( 'NONE',  #14366 ) ;
#9744 = EDGE_LOOP ( 'NONE', ( #13222, #14438, #12105, #12 ) ) ;
#9745 = ORIENTED_EDGE ( 'NONE', *, *, #12861, .T. ) ;
#9746 = VECTOR ( 'NONE', #1354, 1000.000000000000227 ) ;
#9747 = DIRECTION ( 'NONE',  ( -0.9578262852211513190, 0.2873478855663453846, 0.000000000000000000 ) ) ;
#9748 = CLOSED_SHELL ( 'NONE', ( #13335, #13869, #6487, #12147, #5479, #2280, #6986, #2799, #11907, #3306, #1700, #2523, #11955, #1334, #998, #13373, #14490, #11508, #3061, #8720, #10124, #11172, #4528, #6379, #7627, #7097, #4986, #1100, #856, #4408, #9799, #12043 ) ) ;
#9749 = CARTESIAN_POINT ( 'NONE',  ( -4.411504479843656235E-13, -7.790635086498889805, -6.526184258131195293 ) ) ;
#9750 = PLANE ( 'NONE',  #12745 ) ;
#9751 = CARTESIAN_POINT ( 'NONE',  ( 1.500000000000001332, 0.000000000000000000, 0.000000000000000000 ) ) ;
#9752 = UNCERTAINTY_MEASURE_WITH_UNIT (LENGTH_MEASURE( 1.000000000000000082E-05 ), #1212, 'distance_accuracy_value', 'NONE');
#9753 = DIRECTION ( 'NONE',  ( -0.000000000000000000, -0.000000000000000000, -1.000000000000000000 ) ) ;
#9754 = ORIENTED_EDGE ( 'NONE', *, *, #14141, .F. ) ;
#9755 = LINE ( 'NONE', #3032, #379 ) ;
#9756 = LINE ( 'NONE', #736, #1622 ) ;
#9757 = PRODUCT_CONTEXT ( 'NONE', #1779, 'mechanical' ) ;
#9758 = B_SPLINE_CURVE_WITH_KNOTS ( 'NONE', 3,
 ( #12051, #11014, #892, #10950, #2073, #7415 ),
 .UNSPECIFIED., .F., .F.,
 ( 4, 2, 4 ),
 ( 0.004317080428420393828, 0.005486165713042557603, 0.006655250997664721377 ),
 .UNSPECIFIED. ) ;
#9759 = B_SPLINE_CURVE_WITH_KNOTS ( 'NONE', 3,
 ( #14265, #7764, #1998, #12038, #12252 ),
 .UNSPECIFIED., .F., .F.,
 ( 4, 1, 4 ),
 ( 0.000000000000000000, 0.003752776749732568765, 0.007505553499465137529 ),
 .UNSPECIFIED. ) ;
#9760 = CARTESIAN_POINT ( 'NONE',  ( 137.1540310085880776, 355.9707293956415697, -190.0000000000000000 ) ) ;
#9761 = ADVANCED_FACE ( 'NONE', ( #4520 ), #13358, .T. ) ;
#9762 = ORIENTED_EDGE ( 'NONE', *, *, #10343, .F. ) ;
#9763 = EDGE_LOOP ( 'NONE', ( #3371, #10092, #8441, #180 ) ) ;
#9764 = CARTESIAN_POINT ( 'NONE',  ( 1.400000000000000133, 6.245698675651501825E-16, 5.100000000000000533 ) ) ;
#9765 = CARTESIAN_POINT ( 'NONE',  ( 590.0000000000000000, 212.5596934910894333, 210.0000000000000000 ) ) ;
#9766 = EDGE_CURVE ( 'NONE', #2797, #13718, #8334, .T. ) ;
#9767 = CARTESIAN_POINT ( 'NONE',  ( 609.7206935199311602, 188.0285076711449790, -189.0295014234984023 ) ) ;
#9768 = FACE_OUTER_BOUND ( 'NONE', #13738, .T. ) ;
#9769 = VERTEX_POINT ( 'NONE', #3633 ) ;
#9770 = DIRECTION ( 'NONE',  ( -0.000000000000000000, -0.000000000000000000, -1.000000000000000000 ) ) ;
#9771 = ORIENTED_EDGE ( 'NONE', *, *, #6217, .F. ) ;
#9772 = EDGE_CURVE ( 'NONE', #5212, #8286, #1182, .T. ) ;
#9773 = DIRECTION ( 'NONE',  ( -0.000000000000000000, -0.000000000000000000, -1.000000000000000000 ) ) ;
#9774 = DIRECTION ( 'NONE',  ( 0.000000000000000000, 0.000000000000000000, -1.000000000000000000 ) ) ;
#9775 = CARTESIAN_POINT ( 'NONE',  ( -3.999999999999999112, 0.000000000000000000, -7.974599999999998801 ) ) ;
#9776 = ORIENTED_EDGE ( 'NONE', *, *, #935, .F. ) ;
#9777 = CARTESIAN_POINT ( 'NONE',  ( -0.6666666666666666297, -4.233901974057276973, -3.300726591567087365 ) ) ;
#9778 = EDGE_LOOP ( 'NONE', ( #1463, #8398, #5127, #13803 ) ) ;
#9779 = ORIENTED_EDGE ( 'NONE', *, *, #4907, .T. ) ;
#9780 = CARTESIAN_POINT ( 'NONE',  ( 635.0000000000000000, 160.0000000000000284, -211.0000000000000000 ) ) ;
#9781 = CARTESIAN_POINT ( 'NONE',  ( -1.400000000000001910, 0.000000000000000000, 0.000000000000000000 ) ) ;
#9782 = ORIENTED_EDGE ( 'NONE', *, *, #3414, .F. ) ;
#9783 = ORIENTED_EDGE ( 'NONE', *, *, #6189, .T. ) ;
#9784 = DIRECTION ( 'NONE',  ( -0.000000000000000000, 0.000000000000000000, -1.000000000000000000 ) ) ;
#9785 = EDGE_CURVE ( 'NONE', #14483, #11591, #5906, .T. ) ;
#9786 = DIRECTION ( 'NONE',  ( 0.000000000000000000, 0.000000000000000000, -1.000000000000000000 ) ) ;
#9787 = CARTESIAN_POINT ( 'NONE',  ( -0.5636800770129166693, -4.293361309317430319, -3.531542292955206275 ) ) ;
#9788 = DIRECTION ( 'NONE',  ( 0.000000000000000000, 0.000000000000000000, -1.000000000000000000 ) ) ;
#9789 = ORIENTED_EDGE ( 'NONE', *, *, #12037, .F. ) ;
#9790 = DIRECTION ( 'NONE',  ( -1.000000000000000000, 0.000000000000000000, 0.000000000000000000 ) ) ;
#9791 = ITEM_DEFINED_TRANSFORMATION ( 'NONE', 'NONE', #8543,  #9440 ) ;
#9792 = ORIENTED_EDGE ( 'NONE', *, *, #6281, .T. ) ;
#9793 = DIRECTION ( 'NONE',  ( 1.000000000000000000, 0.000000000000000000, -0.000000000000000000 ) ) ;
#9794 = ORIENTED_EDGE ( 'NONE', *, *, #1835, .F. ) ;
#9795 = LINE ( 'NONE', #14516, #4016 ) ;
#9796 = FACE_OUTER_BOUND ( 'NONE', #10944, .T. ) ;
#9797 = VERTEX_POINT ( 'NONE', #11505 ) ;
#9798 = PLANE ( 'NONE',  #10881 ) ;
#9799 = ADVANCED_FACE ( 'NONE', ( #10331 ), #1894, .F. ) ;
#9800 = DIRECTION ( 'NONE',  ( -0.000000000000000000, -0.000000000000000000, -1.000000000000000000 ) ) ;
#9801 = CARTESIAN_POINT ( 'NONE',  ( 153.1991633467111456, 386.6211705227183870, 210.0000000000000000 ) ) ;
#9802 = VERTEX_POINT ( 'NONE', #4883 ) ;
#9803 = EDGE_CURVE ( 'NONE', #12598, #1652, #13878, .T. ) ;
#9804 = DIRECTION ( 'NONE',  ( 9.463134714538378657E-16, -7.093113185993356941E-16, -1.000000000000000000 ) ) ;
#9805 = CARTESIAN_POINT ( 'NONE',  ( 630.0000000000000000, 160.0000000000000284, -210.0000000000000000 ) ) ;
#9806 = ORIENTED_EDGE ( 'NONE', *, *, #12867, .F. ) ;
#9807 =( REPRESENTATION_RELATIONSHIP ('NONE','NONE', #2822, #5933 ) REPRESENTATION_RELATIONSHIP_WITH_TRANSFORMATION ( #559 )SHAPE_REPRESENTATION_RELATIONSHIP( ) );
#9808 = EDGE_CURVE ( 'NONE', #9444, #10436, #3775, .T. ) ;
#9809 = ORIENTED_EDGE ( 'NONE', *, *, #6446, .T. ) ;
#9810 = FACE_OUTER_BOUND ( 'NONE', #14045, .T. ) ;
#9811 = EDGE_CURVE ( 'NONE', #12648, #2165, #220, .T. ) ;
#9812 = DIRECTION ( 'NONE',  ( -0.000000000000000000, 0.000000000000000000, -1.000000000000000000 ) ) ;
#9813 = ADVANCED_FACE ( 'NONE', ( #10415 ), #279, .F. ) ;
#9814 = CYLINDRICAL_SURFACE ( 'NONE', #9697, 4.199999999999926459 ) ;
#9815 = CARTESIAN_POINT ( 'NONE',  ( 629.0000000000000000, 166.0000000000000284, -187.5000000000000000 ) ) ;
#9816 = CARTESIAN_POINT ( 'NONE',  ( -6.815830331203685866, -0.6619522098568484392, -6.171384342982615401 ) ) ;
#9817 = ORIENTED_EDGE ( 'NONE', *, *, #13661, .T. ) ;
#9818 = LINE ( 'NONE', #5322, #862 ) ;
#9819 = DIRECTION ( 'NONE',  ( 1.000000000000000000, 0.000000000000000000, 0.000000000000000000 ) ) ;
#9820 = DIRECTION ( 'NONE',  ( 0.000000000000000000, 0.000000000000000000, -1.000000000000000000 ) ) ;
#9821 = EDGE_CURVE ( 'NONE', #6337, #9054, #10145, .T. ) ;
#9822 = ADVANCED_FACE ( 'NONE', ( #4956 ), #13378, .F. ) ;
#9823 = FACE_OUTER_BOUND ( 'NONE', #2723, .T. ) ;
#9824 = ORIENTED_EDGE ( 'NONE', *, *, #11544, .F. ) ;
#9825 = EDGE_LOOP ( 'NONE', ( #8025, #10564 ) ) ;
#9826 = DIRECTION ( 'NONE',  ( 0.000000000000000000, -0.000000000000000000, 1.000000000000000000 ) ) ;
#9827 = FACE_OUTER_BOUND ( 'NONE', #11434, .T. ) ;
#9828 = EDGE_CURVE ( 'NONE', #6153, #4085, #9830, .T. ) ;
#9829 = CARTESIAN_POINT ( 'NONE',  ( 6.207671477328661425, 5.338259717474330479, 0.7538629453361838095 ) ) ;
#9830 = LINE ( 'NONE', #8866, #8489 ) ;
#9831 = VERTEX_POINT ( 'NONE', #14482 ) ;
#9832 = CARTESIAN_POINT ( 'NONE',  ( 642.0000000000000000, 167.0000000000000000, -225.5000000000000000 ) ) ;
#9833 = ORIENTED_EDGE ( 'NONE', *, *, #8085, .F. ) ;
#9834 = CIRCLE ( 'NONE', #2312, 2.199999999999711520 ) ;
#9835 = VECTOR ( 'NONE', #4076, 1000.000000000000000 ) ;
#9836 = AXIS2_PLACEMENT_3D ( 'NONE', #1343, #3648, #7102 ) ;
#9837 = LINE ( 'NONE', #7633, #5618 ) ;
#9838 = DIRECTION ( 'NONE',  ( 1.000000000000000000, 2.312964634635740689E-15, 0.000000000000000000 ) ) ;
#9839 = CARTESIAN_POINT ( 'NONE',  ( 610.0000000000000000, 227.4403065089105951, 187.0000000000000000 ) ) ;
#9840 = ORIENTED_EDGE ( 'NONE', *, *, #7567, .F. ) ;
#9841 = LINE ( 'NONE', #4238, #1887 ) ;
#9842 = EDGE_LOOP ( 'NONE', ( #4151, #1982, #9266, #2051 ) ) ;
#9843 = EDGE_LOOP ( 'NONE', ( #6277, #8529, #10155, #4737, #5159, #6234 ) ) ;
#9844 = CARTESIAN_POINT ( 'NONE',  ( 0.000000000000000000, 4.330127018922190985, -2.500000000000007105 ) ) ;
#9845 = VECTOR ( 'NONE', #3768, 1000.000000000000000 ) ;
#9846 = DIRECTION ( 'NONE',  ( 0.2873478855663448850, 0.9578262852211515410, -3.408579461568462910E-15 ) ) ;
#9847 = VECTOR ( 'NONE', #13178, 1000.000000000000227 ) ;
#9848 = VERTEX_POINT ( 'NONE', #4303 ) ;
#9849 = VERTEX_POINT ( 'NONE', #4438 ) ;
#9850 = CARTESIAN_POINT ( 'NONE',  ( 0.000000000000000000, 0.000000000000000000, 0.000000000000000000 ) ) ;
#9851 = LINE ( 'NONE', #12132, #9900 ) ;
#9852 = CARTESIAN_POINT ( 'NONE',  ( 130.2060951089103185, 434.0203170297010615, -190.0000000000001990 ) ) ;
#9853 = FACE_OUTER_BOUND ( 'NONE', #11092, .T. ) ;
#9854 = VERTEX_POINT ( 'NONE', #5482 ) ;
#9855 = AXIS2_PLACEMENT_3D ( 'NONE', #10867, #7244, #11731 ) ;
#9856 = CARTESIAN_POINT ( 'NONE',  ( 610.0000000000000000, 227.4403065089105951, 187.0000000000000000 ) ) ;
#9857 = ITEM_DEFINED_TRANSFORMATION ( 'NONE', 'NONE', #3602,  #9440 ) ;
#9858 = CIRCLE ( 'NONE', #408, 4.000000000000000000 ) ;
#9859 = EDGE_LOOP ( 'NONE', ( #16, #5492, #7296, #1509 ) ) ;
#9860 = DIRECTION ( 'NONE',  ( 0.9578262852211514300, -0.2873478855663454401, 0.000000000000000000 ) ) ;
#9861 = ORIENTED_EDGE ( 'NONE', *, *, #4054, .T. ) ;
#9862 = EDGE_CURVE ( 'NONE', #3037, #3179, #14412, .T. ) ;
#9863 = CARTESIAN_POINT ( 'NONE',  ( -6.500000000000000000, 3.752776749732564809, -0.7999999999999969358 ) ) ;
#9864 = CYLINDRICAL_SURFACE ( 'NONE', #6400, 2.199999999999701306 ) ;
#9865 = AXIS2_PLACEMENT_3D ( 'NONE', #370, #305, #13911 ) ;
#9866 = CONICAL_SURFACE ( 'NONE', #4661, 3.309499999999999886, 0.7853981633974407295 ) ;
#9867 = EDGE_LOOP ( 'NONE', ( #10444, #14335, #7497, #2388 ) ) ;
#9868 = CARTESIAN_POINT ( 'NONE',  ( 641.0000000000000000, 166.0000000000000284, -187.5000000000000000 ) ) ;
#9869 = PLANE ( 'NONE',  #11759 ) ;
#9870 = CARTESIAN_POINT ( 'NONE',  ( 611.4942090049451053, 232.4210031920599420, -184.7999999999999829 ) ) ;
#9871 = ORIENTED_EDGE ( 'NONE', *, *, #9113, .F. ) ;
#9872 = AXIS2_PLACEMENT_3D ( 'NONE', #6292, #14340, #9913 ) ;
#9873 = LINE ( 'NONE', #14380, #14375 ) ;
#9874 = VERTEX_POINT ( 'NONE', #11222 ) ;
#9875 = CIRCLE ( 'NONE', #12694, 6.750000000000000000 ) ;
#9876 = VERTEX_POINT ( 'NONE', #4226 ) ;
#9877 = CARTESIAN_POINT ( 'NONE',  ( -0.04050535873993951069, -7.919512791578242172, -6.573129608219095310 ) ) ;
#9878 = EDGE_CURVE ( 'NONE', #5738, #5202, #8726, .T. ) ;
#9879 = DIRECTION ( 'NONE',  ( 1.000000000000000000, 0.000000000000000000, 0.000000000000000000 ) ) ;
#9880 = VECTOR ( 'NONE', #8694, 1000.000000000000000 ) ;
#9881 = CARTESIAN_POINT ( 'NONE',  ( 627.6903011687218168, 161.9515302464737943, -210.0000000000000000 ) ) ;
#9882 = LINE ( 'NONE', #12020, #12035 ) ;
#9883 = EDGE_CURVE ( 'NONE', #1138, #5518, #5669, .T. ) ;
#9884 = CIRCLE ( 'NONE', #2332, 0.7499999999999997780 ) ;
#9885 = EDGE_CURVE ( 'NONE', #2876, #3186, #721, .T. ) ;
#9886 = AXIS2_PLACEMENT_3D ( 'NONE', #3225, #2941, #8774 ) ;
#9887 = UNCERTAINTY_MEASURE_WITH_UNIT (LENGTH_MEASURE( 1.000000000000000082E-05 ), #4840, 'distance_accuracy_value', 'NONE');
#9888 = CARTESIAN_POINT ( 'NONE',  ( 3.500000000000000000, -2.309401076758502480, -4.000000000000000000 ) ) ;
#9889 = EDGE_LOOP ( 'NONE', ( #4342, #917, #7777, #23 ) ) ;
#9890 = EDGE_CURVE ( 'NONE', #1912, #9874, #12111, .T. ) ;
#9891 = CARTESIAN_POINT ( 'NONE',  ( 0.000000000000000000, -1.178949249685214307, 2.042000000000001592 ) ) ;
#9892 = CARTESIAN_POINT ( 'NONE',  ( -3.309651814758565180, -5.455921364805393026, -1.000000000000000000 ) ) ;
#9893 = AXIS2_PLACEMENT_3D ( 'NONE', #9061, #7054, #5740 ) ;
#9894 = CARTESIAN_POINT ( 'NONE',  ( 2.999999999999999112, 4.618802153517012954, 0.000000000000000000 ) ) ;
#9895 = ORIENTED_EDGE ( 'NONE', *, *, #6752, .T. ) ;
#9896 = ORIENTED_EDGE ( 'NONE', *, *, #8285, .T. ) ;
#9897 = SURFACE_SIDE_STYLE ('',( #14478 ) ) ;
#9898 = CARTESIAN_POINT ( 'NONE',  ( -3.250000000000003997, -5.629165124598849879, 0.000000000000000000 ) ) ;
#9899 = AXIS2_PLACEMENT_3D ( 'NONE', #12225, #1986, #14527 ) ;
#9900 = VECTOR ( 'NONE', #2016, 1000.000000000000000 ) ;
#9901 = LINE ( 'NONE', #2141, #13897 ) ;
#9902 = AXIS2_PLACEMENT_3D ( 'NONE', #4660, #12391, #2360 ) ;
#9903 = FACE_OUTER_BOUND ( 'NONE', #10709, .T. ) ;
#9904 = AXIS2_PLACEMENT_3D ( 'NONE', #2007, #6522, #6459 ) ;
#9905 = ORIENTED_EDGE ( 'NONE', *, *, #11721, .T. ) ;
#9906 = EDGE_CURVE ( 'NONE', #11133, #1120, #9759, .T. ) ;
#9907 = FACE_OUTER_BOUND ( 'NONE', #5760, .T. ) ;
#9908 = EDGE_LOOP ( 'NONE', ( #1631, #14498, #11332, #315, #4426 ) ) ;
#9909 = CONICAL_SURFACE ( 'NONE', #8732, 6.500000000000000888, 0.8987552595851582282 ) ;
#9910 = EDGE_CURVE ( 'NONE', #13338, #9269, #13690, .T. ) ;
#9911 = TOROIDAL_SURFACE ( 'NONE', #3078, 6.250000000000000000, 0.7500000000000000000 ) ;
#9912 = CARTESIAN_POINT ( 'NONE',  ( -8.505790995054926640, 376.6597771564183859, -187.0000000000000000 ) ) ;
#9913 = DIRECTION ( 'NONE',  ( 1.000000000000000000, 0.000000000000000000, 0.000000000000000000 ) ) ;
#9914 = DIRECTION ( 'NONE',  ( 0.000000000000000000, -1.000000000000000000, 3.674212649225140308E-15 ) ) ;
#9915 = FILL_AREA_STYLE ('',( #6294 ) ) ;
#9916 = EDGE_LOOP ( 'NONE', ( #83, #12727, #13327, #4094, #9167 ) ) ;
#9917 = DIRECTION ( 'NONE',  ( 0.000000000000000000, -1.000000000000000000, 0.000000000000000000 ) ) ;
#9918 = ORIENTED_EDGE ( 'NONE', *, *, #9069, .F. ) ;
#9919 = ORIENTED_EDGE ( 'NONE', *, *, #12774, .T. ) ;
#9920 = VECTOR ( 'NONE', #5466, 1000.000000000000227 ) ;
#9921 = CARTESIAN_POINT ( 'NONE',  ( 446.3084422793565409, 264.0194060144110608, -187.0000000000000000 ) ) ;
#9922 = AXIS2_PLACEMENT_3D ( 'NONE', #441, #4971, #213 ) ;
#9923 = PLANE ( 'NONE',  #8697 ) ;
#9924 = VECTOR ( 'NONE', #3025, 1000.000000000000000 ) ;
#9925 =( GEOMETRIC_REPRESENTATION_CONTEXT ( 3 ) GLOBAL_UNCERTAINTY_ASSIGNED_CONTEXT ( ( #7527 ) ) GLOBAL_UNIT_ASSIGNED_CONTEXT ( ( #13846, #11848, #5078 ) ) REPRESENTATION_CONTEXT ( 'NONE', 'WORKASPACE' ) );
#9926 = LINE ( 'NONE', #12058, #4042 ) ;
#9927 = ORIENTED_EDGE ( 'NONE', *, *, #8633, .F. ) ;
#9928 = AXIS2_PLACEMENT_3D ( 'NONE', #4565, #8900, #3381 ) ;
#9929 = EDGE_LOOP ( 'NONE', ( #13977, #4021 ) ) ;
#9930 = FACE_BOUND ( 'NONE', #5587, .T. ) ;
#9931 = CARTESIAN_POINT ( 'NONE',  ( 708.1388811837595085, 164.7984674554473941, 177.6000000000000512 ) ) ;
#9932 = AXIS2_PLACEMENT_3D ( 'NONE', #7798, #13113, #7499 ) ;
#9933 = DIRECTION ( 'NONE',  ( 0.000000000000000000, 0.000000000000000000, 1.000000000000000000 ) ) ;
#9934 = PLANE ( 'NONE',  #8423 ) ;
#9935 = CARTESIAN_POINT ( 'NONE',  ( 635.0000000000000000, 160.0000000000000284, 187.5000000000000000 ) ) ;
#9936 =( LENGTH_UNIT ( ) NAMED_UNIT ( * ) SI_UNIT ( .MILLI., .METRE. ) );
#9937 = ORIENTED_EDGE ( 'NONE', *, *, #7645, .F. ) ;
#9938 = VECTOR ( 'NONE', #10972, 1000.000000000000000 ) ;
#9939 = CARTESIAN_POINT ( 'NONE',  ( 609.6990795428844194, 187.6157354204721912, 188.7107384553189888 ) ) ;
#9940 = EDGE_LOOP ( 'NONE', ( #13056, #13915, #10681, #8102 ) ) ;
#9941 = CARTESIAN_POINT ( 'NONE',  ( 21.00000000000000000, 2.055000000000000160, 0.000000000000000000 ) ) ;
#9942 = EDGE_CURVE ( 'NONE', #1456, #7897, #6449, .T. ) ;
#9943 = ORIENTED_EDGE ( 'NONE', *, *, #7979, .F. ) ;
#9944 = AXIS2_PLACEMENT_3D ( 'NONE', #6834, #11409, #5580 ) ;
#9945 = EDGE_CURVE ( 'NONE', #12403, #8156, #7088, .T. ) ;
#9946 = CARTESIAN_POINT ( 'NONE',  ( 610.0000000000000000, 175.0000000000000568, -210.0000000000000000 ) ) ;
#9947 = DIRECTION ( 'NONE',  ( 0.000000000000000000, 0.000000000000000000, 1.000000000000000000 ) ) ;
#9948 = STYLED_ITEM ( 'NONE', ( #10047 ), #4558 ) ;
#9949 = ORIENTED_EDGE ( 'NONE', *, *, #5113, .T. ) ;
#9950 = DIRECTION ( 'NONE',  ( -0.9578262852211513190, 0.2873478855663453846, 0.000000000000000000 ) ) ;
#9951 = FACE_OUTER_BOUND ( 'NONE', #3347, .T. ) ;
#9952 = DIRECTION ( 'NONE',  ( 0.000000000000000000, -1.224646799147353454E-16, 1.000000000000000000 ) ) ;
#9953 = CONICAL_SURFACE ( 'NONE', #1468, 3.339999999999998970, 0.9599310885968821427 ) ;
#9954 = ORIENTED_EDGE ( 'NONE', *, *, #11146, .F. ) ;
#9956 = EDGE_CURVE ( 'NONE', #12648, #7989, #3344, .T. ) ;
#9955 = DIRECTION ( 'NONE',  ( -1.000000000000000000, 0.000000000000000000, -1.063400795443704616E-15 ) ) ;
#9957 = ORIENTED_EDGE ( 'NONE', *, *, #7563, .F. ) ;
#9958 = AXIS2_PLACEMENT_3D ( 'NONE', #10561, #3568, #3710 ) ;
#9959 = ORIENTED_EDGE ( 'NONE', *, *, #11307, .T. ) ;
#9960 = CARTESIAN_POINT ( 'NONE',  ( 1.399999999999998579, 0.000000000000000000, 0.000000000000000000 ) ) ;
#9961 = CARTESIAN_POINT ( 'NONE',  ( 133.6739427831727198, 370.3381236739588758, 210.0000000000000000 ) ) ;
#9962 = VECTOR ( 'NONE', #2930, 1000.000000000000000 ) ;
#9963 = CARTESIAN_POINT ( 'NONE',  ( 4.000000000000000000, -1.942223658245635809, -0.3516579909967643691 ) ) ;
#9964 = CARTESIAN_POINT ( 'NONE',  ( 610.0000000000000000, 145.0000000000000568, -190.0000000000000000 ) ) ;
#9965 = CARTESIAN_POINT ( 'NONE',  ( 4.444974277457895973, 4.939246403833855936, -5.720331885005371042 ) ) ;
#9966 = CARTESIAN_POINT ( 'NONE',  ( -3.098410542199071749, -7.060458129626440815, 0.000000000000000000 ) ) ;
#9967 = ADVANCED_FACE ( 'NONE', ( #882, #9903 ), #5404, .T. ) ;
#9968 = ORIENTED_EDGE ( 'NONE', *, *, #11668, .T. ) ;
#9969 = CARTESIAN_POINT ( 'NONE',  ( 455.5035746174796714, 294.6698471414878782, 210.0000000000000000 ) ) ;
#9970 = CARTESIAN_POINT ( 'NONE',  ( 6.385552186430389909, -5.773502691896264416, 3.657698248296050164E-17 ) ) ;
#9971 = PRODUCT_CONTEXT ( 'NONE', #14615, 'mechanical' ) ;
#9973 = AXIS2_PLACEMENT_3D ( 'NONE', #8509, #13234, #967 ) ;
#9972 = CARTESIAN_POINT ( 'NONE',  ( -6.500000000000000000, 2.501851166488374911, -5.848636054922034866 ) ) ;
#9974 = ORIENTED_EDGE ( 'NONE', *, *, #9115, .T. ) ;
#9975 = EDGE_LOOP ( 'NONE', ( #5790, #8831, #6663, #129 ) ) ;
#9976 = DIRECTION ( 'NONE',  ( 1.000000000000000000, 0.000000000000000000, 0.000000000000000000 ) ) ;
#9977 = CARTESIAN_POINT ( 'NONE',  ( 4.211140560182196957, 2.431303136016536470, -3.745885042887433514 ) ) ;
#9978 = CARTESIAN_POINT ( 'NONE',  ( 2.832728918602883006, 6.234773369952725020, -6.171481112545252223 ) ) ;
#9979 = ORIENTED_EDGE ( 'NONE', *, *, #5569, .F. ) ;
#9980 = SHAPE_REPRESENTATION ( 'hub', ( #9440 ), #9925 ) ;
#9981 = DIRECTION ( 'NONE',  ( -0.000000000000000000, 0.000000000000000000, -1.000000000000000000 ) ) ;
#9982 = EDGE_CURVE ( 'NONE', #3582, #12176, #3774, .T. ) ;
#9983 = ORIENTED_EDGE ( 'NONE', *, *, #5250, .F. ) ;
#9984 = CARTESIAN_POINT ( 'NONE',  ( 148.9991633467111569, 386.6211705227183870, -187.0000000000000568 ) ) ;
#9985 = LINE ( 'NONE', #7072, #2329 ) ;
#9986 = DIRECTION ( 'NONE',  ( -0.000000000000000000, -0.000000000000000000, 1.000000000000000000 ) ) ;
#9987 = FACE_OUTER_BOUND ( 'NONE', #13866, .T. ) ;
#9988 = ORIENTED_EDGE ( 'NONE', *, *, #12408, .F. ) ;
#9989 = EDGE_LOOP ( 'NONE', ( #8213, #2579, #207, #6321 ) ) ;
#9990 = EDGE_CURVE ( 'NONE', #6163, #2855, #14322, .T. ) ;
#9991 = CARTESIAN_POINT ( 'NONE',  ( 610.0000000000000000, 227.4403065089105951, -187.0000000000000000 ) ) ;
#9992 = ADVANCED_FACE ( 'NONE', ( #1485 ), #10266, .F. ) ;
#9993 = LINE ( 'NONE', #10212, #8214 ) ;
#9994 = EDGE_CURVE ( 'NONE', #12104, #8752, #5910, .T. ) ;
#9995 = DIRECTION ( 'NONE',  ( 1.000000000000000000, 0.000000000000000000, 0.000000000000000000 ) ) ;
#9996 = VERTEX_POINT ( 'NONE', #12394 ) ;
#9997 = VERTEX_POINT ( 'NONE', #10334 ) ;
#9998 = CARTESIAN_POINT ( 'NONE',  ( 2.500000000000000000, 0.000000000000000000, 0.000000000000000000 ) ) ;
#9999 = CARTESIAN_POINT ( 'NONE',  ( 1.312671235360372224, 3.860931062424219462, -0.05923475698270440348 ) ) ;
#10000 = CARTESIAN_POINT ( 'NONE',  ( 637.0568832135862749, 155.4426727739092655, 215.5000000000000000 ) ) ;
#10001 = CARTESIAN_POINT ( 'NONE',  ( 636.7009106935324780, 155.5114698605638637, -210.0000000000000000 ) ) ;
#10002 = DIRECTION ( 'NONE',  ( -1.000000000000000000, 0.000000000000000000, 0.000000000000000000 ) ) ;
#10003 = ORIENTED_EDGE ( 'NONE', *, *, #8081, .F. ) ;
#10004 = SURFACE_SIDE_STYLE ('',( #11915 ) ) ;
#10005 = CONTEXT_DEPENDENT_SHAPE_REPRESENTATION ( #14143, #9729 ) ;
#10006 = EDGE_LOOP ( 'NONE', ( #2658, #6371 ) ) ;
#10007 = ORIENTED_EDGE ( 'NONE', *, *, #9069, .T. ) ;
#10008 = FACE_OUTER_BOUND ( 'NONE', #6619, .T. ) ;
#10009 = EDGE_CURVE ( 'NONE', #2837, #6163, #2338, .T. ) ;
#10010 = ORIENTED_EDGE ( 'NONE', *, *, #7715, .F. ) ;
#10011 = DIRECTION ( 'NONE',  ( 1.000000000000000000, 0.000000000000000000, 0.000000000000000000 ) ) ;
#10012 = DIRECTION ( 'NONE',  ( 0.000000000000000000, 0.000000000000000000, 1.000000000000000000 ) ) ;
#10013 = ORIENTED_EDGE ( 'NONE', *, *, #1858, .F. ) ;
#10014 = DIRECTION ( 'NONE',  ( 1.000000000000000000, 0.000000000000000000, 0.000000000000000000 ) ) ;
#10015 = DIRECTION ( 'NONE',  ( 0.000000000000000000, 0.000000000000000000, 1.000000000000000000 ) ) ;
#10016 = EDGE_CURVE ( 'NONE', #3125, #7721, #7009, .T. ) ;
#10017 = CARTESIAN_POINT ( 'NONE',  ( 708.1388811837593948, 164.7984674554466835, -177.6000000000002217 ) ) ;
#10018 = ORIENTED_EDGE ( 'NONE', *, *, #4561, .F. ) ;
#10019 = ADVANCED_FACE ( 'NONE', ( #9086 ), #12693, .F. ) ;
#10020 = ORIENTED_EDGE ( 'NONE', *, *, #791, .T. ) ;
#10021 = ORIENTED_EDGE ( 'NONE', *, *, #2425, .F. ) ;
#10022 = DIRECTION ( 'NONE',  ( 1.000000000000000000, 0.000000000000000000, 0.000000000000000000 ) ) ;
#10023 = DIRECTION ( 'NONE',  ( 9.794481010665704304E-16, 3.264827003555233190E-15, 1.000000000000000000 ) ) ;
#10024 = CARTESIAN_POINT ( 'NONE',  ( 2.500000000000000000, -1.178949249685214307, 2.042000000000001592 ) ) ;
#10025 = CARTESIAN_POINT ( 'NONE',  ( 0.4465819873851989974, -2.886751345948121106, 4.999999999999999112 ) ) ;
#10026 = CARTESIAN_POINT ( 'NONE',  ( -8.505790995054828940, 418.4210031920615620, -184.7999999999999829 ) ) ;
#10027 = CARTESIAN_POINT ( 'NONE',  ( 455.5035746174796714, 294.6698471414878782, -210.0000000000000000 ) ) ;
#10028 = DIRECTION ( 'NONE',  ( -1.000000000000000000, 0.000000000000000000, 0.000000000000000000 ) ) ;
#10029 = ORIENTED_EDGE ( 'NONE', *, *, #12749, .T. ) ;
#10030 = ADVANCED_BREP_SHAPE_REPRESENTATION ( '', ( #2215, #9440 ), #2396 ) ;
#10031 = LINE ( 'NONE', #14536, #5825 ) ;
#10032 = LINE ( 'NONE', #10256, #12454 ) ;
#10033 = PRODUCT_CONTEXT ( 'NONE', #14428, 'mechanical' ) ;
#10034 = LINE ( 'NONE', #3248, #8969 ) ;
#10035 = VERTEX_POINT ( 'NONE', #10200 ) ;
#10036 = EDGE_LOOP ( 'NONE', ( #3571, #1524 ) ) ;
#10037 = PRESENTATION_STYLE_ASSIGNMENT (( #12245 ) ) ;
#10038 = FACE_OUTER_BOUND ( 'NONE', #7583, .T. ) ;
#10039 = CARTESIAN_POINT ( 'NONE',  ( -6.080745460913608902, 0.5192545390863924082, -1.000000000000000000 ) ) ;
#10040 = ADVANCED_FACE ( 'NONE', ( #1331 ), #11297, .F. ) ;
#10041 = CARTESIAN_POINT ( 'NONE',  ( -2.075968632161309557, 6.306992450857741517, -6.056431503346038525 ) ) ;
#10042 = EDGE_LOOP ( 'NONE', ( #9607, #7727, #12638, #9651 ) ) ;
#10043 = LINE ( 'NONE', #2282, #13034 ) ;
#10044 = VERTEX_POINT ( 'NONE', #1183 ) ;
#10045 = LINE ( 'NONE', #6518, #9147 ) ;
#10046 = DIRECTION ( 'NONE',  ( 1.000000000000000000, 0.000000000000000000, 0.000000000000000000 ) ) ;
#10047 = PRESENTATION_STYLE_ASSIGNMENT (( #11229 ) ) ;
#10048 = CARTESIAN_POINT ( 'NONE',  ( 6.196878017913830305, 3.367876570272813730, 4.166666666666666075 ) ) ;
#10049 = ORIENTED_EDGE ( 'NONE', *, *, #9193, .T. ) ;
#10050 = VERTEX_POINT ( 'NONE', #125 ) ;
#10051 = CARTESIAN_POINT ( 'NONE',  ( 631.0000000000000000, 164.0000000000000284, -233.5000000000000000 ) ) ;
#10052 = CARTESIAN_POINT ( 'NONE',  ( 1.600000000000000089, 3.306546357697853733E-16, -2.700000000000000178 ) ) ;
#10053 = AXIS2_PLACEMENT_3D ( 'NONE', #9888, #14393, #8789 ) ;
#10054 = EDGE_CURVE ( 'NONE', #3531, #852, #2589, .T. ) ;
#10055 = DIRECTION ( 'NONE',  ( 1.000000000000000000, 0.000000000000000000, 0.000000000000000000 ) ) ;
#10056 = EDGE_CURVE ( 'NONE', #1708, #13276, #8741, .T. ) ;
#10057 = ORIENTED_EDGE ( 'NONE', *, *, #12495, .F. ) ;
#10058 = VECTOR ( 'NONE', #14254, 1000.000000000000000 ) ;
#10059 = AXIS2_PLACEMENT_3D ( 'NONE', #1798, #11906, #12953 ) ;
#10060 = ORIENTED_EDGE ( 'NONE', *, *, #3848, .T. ) ;
#10061 = CARTESIAN_POINT ( 'NONE',  ( 609.7814593570623174, 185.8554382275811463, -186.1689414351991161 ) ) ;
#10062 = CARTESIAN_POINT ( 'NONE',  ( 610.0000000000000000, 145.0000000000000568, 190.0000000000000000 ) ) ;
#10063 = EDGE_CURVE ( 'NONE', #14073, #8007, #2281, .T. ) ;
#10064 = CARTESIAN_POINT ( 'NONE',  ( -2.354826896168714434, -6.962563485461402024, -1.000000000000000000 ) ) ;
#10065 = CARTESIAN_POINT ( 'NONE',  ( -0.3208286057739654917, 4.433571671609680465, -0.3503314178412548774 ) ) ;
#10066 = CARTESIAN_POINT ( 'NONE',  ( 0.3572655899080433572, -2.309401076758680116, -4.000000000000000000 ) ) ;
#10067 = ORIENTED_EDGE ( 'NONE', *, *, #9956, .F. ) ;
#10068 = EDGE_CURVE ( 'NONE', #12479, #7181, #13586, .T. ) ;
#10069 = DIRECTION ( 'NONE',  ( -0.2873478855663453846, -0.9578262852211513190, -0.000000000000000000 ) ) ;
#10070 = VERTEX_POINT ( 'NONE', #2444 ) ;
#10071 = VERTEX_POINT ( 'NONE', #7089 ) ;
#10072 = DIRECTION ( 'NONE',  ( -0.000000000000000000, -0.000000000000000000, -1.000000000000000000 ) ) ;
#10073 = EDGE_LOOP ( 'NONE', ( #7435, #9436, #6983, #1408, #6746 ) ) ;
#10074 = VECTOR ( 'NONE', #11612, 1000.000000000000000 ) ;
#10075 = VECTOR ( 'NONE', #3783, 1000.000000000000000 ) ;
#10076 = DIRECTION ( 'NONE',  ( -1.000000000000000000, -0.000000000000000000, -0.000000000000000000 ) ) ;
#10077 = APPLICATION_CONTEXT ( 'automotive_design' ) ;
#10078 = DIRECTION ( 'NONE',  ( 0.000000000000000000, 0.000000000000000000, -1.000000000000000000 ) ) ;
#10079 = ORIENTED_EDGE ( 'NONE', *, *, #11307, .F. ) ;
#10080 = CARTESIAN_POINT ( 'NONE',  ( -8.505790995054768544, 418.4210031920615620, -184.7999999999999829 ) ) ;
#10081 = DIRECTION ( 'NONE',  ( -1.000000000000000000, 0.000000000000000000, 0.000000000000000000 ) ) ;
#10082 = ADVANCED_FACE ( 'NONE', ( #5698 ), #60, .T. ) ;
#10083 = AXIS2_PLACEMENT_3D ( 'NONE', #742, #4152, #8644 ) ;
#10084 = EDGE_CURVE ( 'NONE', #8076, #6357, #12500, .T. ) ;
#10085 = VECTOR ( 'NONE', #5718, 1000.000000000000000 ) ;
#10086 = CARTESIAN_POINT ( 'NONE',  ( -9.498873539028489220E-16, 10.00000000000000000, -210.0000000000000000 ) ) ;
#10087 = DIRECTION ( 'NONE',  ( 0.000000000000000000, 0.000000000000000000, -1.000000000000000000 ) ) ;
#10088 = FILL_AREA_STYLE ('',( #2191 ) ) ;
#10089 = ORIENTED_EDGE ( 'NONE', *, *, #9438, .F. ) ;
#10090 = EDGE_CURVE ( 'NONE', #54, #14275, #1267, .T. ) ;
#10091 = DIRECTION ( 'NONE',  ( -0.000000000000000000, -0.000000000000000000, 1.000000000000000000 ) ) ;
#10092 = ORIENTED_EDGE ( 'NONE', *, *, #10433, .F. ) ;
#10093 = VERTEX_POINT ( 'NONE', #7167 ) ;
#10094 = DIRECTION ( 'NONE',  ( -0.9578262852211513190, 0.2873478855663453846, 0.000000000000000000 ) ) ;
#10095 = AXIS2_PLACEMENT_3D ( 'NONE', #7445, #1617, #10631 ) ;
#10097 = CIRCLE ( 'NONE', #11977, 5.199999999999999289 ) ;
#10096 = DIRECTION ( 'NONE',  ( 1.000000000000000000, 0.000000000000000000, 0.000000000000000000 ) ) ;
#10098 = CONICAL_SURFACE ( 'NONE', #7498, 3.339999999999998970, 0.9599310885968821427 ) ;
#10099 = DIRECTION ( 'NONE',  ( -1.000000000000000000, -0.000000000000000000, 0.000000000000000000 ) ) ;
#10100 = CARTESIAN_POINT ( 'NONE',  ( 451.3035746174797396, 294.6698471414878782, -190.0000000000000000 ) ) ;
#10101 = CARTESIAN_POINT ( 'NONE',  ( 0.000000000000000000, 0.000000000000000000, 0.000000000000000000 ) ) ;
#10102 = FACE_BOUND ( 'NONE', #11103, .T. ) ;
#10103 = CARTESIAN_POINT ( 'NONE',  ( 0.000000000000000000, 0.000000000000000000, 0.000000000000000000 ) ) ;
#10104 = ORIENTED_EDGE ( 'NONE', *, *, #2136, .T. ) ;
#10105 = VECTOR ( 'NONE', #10609, 1000.000000000000000 ) ;
#10106 = VECTOR ( 'NONE', #7429, 1000.000000000000000 ) ;
#10107 = DIRECTION ( 'NONE',  ( 0.000000000000000000, 1.000000000000000000, 0.000000000000000000 ) ) ;
#10108 = DIRECTION ( 'NONE',  ( 1.416419855379454792E-15, -4.619333907680102023E-16, -1.000000000000000000 ) ) ;
#10109 = PRODUCT_CONTEXT ( 'NONE', #3590, 'mechanical' ) ;
#10110 = DIRECTION ( 'NONE',  ( 0.000000000000000000, 0.000000000000000000, -1.000000000000000000 ) ) ;
#10111 = ORIENTED_EDGE ( 'NONE', *, *, #4561, .T. ) ;
#10112 = EDGE_LOOP ( 'NONE', ( #5934, #174, #7377, #14117 ) ) ;
#10113 = CARTESIAN_POINT ( 'NONE',  ( 229.2257385731833779, 308.4724102386176128, -179.7999999999999545 ) ) ;
#10114 = AXIS2_PLACEMENT_3D ( 'NONE', #5338, #2003, #6456 ) ;
#10115 = DIRECTION ( 'NONE',  ( 0.9396926207859138680, 1.150791560227856926E-16, -0.3420201433256536139 ) ) ;
#10116 = CIRCLE ( 'NONE', #3055, 7.500000000000000000 ) ;
#10117 = AXIS2_PLACEMENT_3D ( 'NONE', #6912, #13623, #3301 ) ;
#10118 = CARTESIAN_POINT ( 'NONE',  ( 0.2494252716035016415, 1.935831255942371154, 3.999999999999993339 ) ) ;
#10119 = CARTESIAN_POINT ( 'NONE',  ( 6.390983399715594260, -5.837459000499770845, 0.1107755759658283073 ) ) ;
#10120 = ORIENTED_EDGE ( 'NONE', *, *, #12700, .T. ) ;
#10121 = VECTOR ( 'NONE', #1080, 999.9999999999998863 ) ;
#10122 = DIRECTION ( 'NONE',  ( -0.9578262852211507639, 0.2873478855663477716, 0.000000000000000000 ) ) ;
#10123 = CYLINDRICAL_SURFACE ( 'NONE', #2078, 4.199999999999926459 ) ;
#10124 = ADVANCED_FACE ( 'NONE', ( #12918 ), #6149, .T. ) ;
#10125 = AXIS2_PLACEMENT_3D ( 'NONE', #6768, #7604, #12306 ) ;
#10126 = CARTESIAN_POINT ( 'NONE',  ( 0.2500000000000002220, 0.000000000000000000, 0.000000000000000000 ) ) ;
#10127 = CIRCLE ( 'NONE', #1416, 7.500000000000062172 ) ;
#10128 = EDGE_CURVE ( 'NONE', #1845, #4375, #3990, .T. ) ;
#10129 = VERTEX_POINT ( 'NONE', #9675 ) ;
#10130 = ORIENTED_EDGE ( 'NONE', *, *, #1586, .T. ) ;
#10131 = CARTESIAN_POINT ( 'NONE',  ( 42.80949999999999278, 0.000000000000000000, 4.000000000000000000 ) ) ;
#10132 = DIRECTION ( 'NONE',  ( 0.000000000000000000, 0.000000000000000000, 1.000000000000000000 ) ) ;
#10133 = CIRCLE ( 'NONE', #6410, 5.249999999999976907 ) ;
#10134 = AXIS2_PLACEMENT_3D ( 'NONE', #3661, #4993, #8297 ) ;
#10135 = FACE_OUTER_BOUND ( 'NONE', #7702, .T. ) ;
#10136 = TOROIDAL_SURFACE ( 'NONE', #6142, 8.331345277524542681, 0.6186547224754559426 ) ;
#10137 = VERTEX_POINT ( 'NONE', #14033 ) ;
#10138 = VECTOR ( 'NONE', #12677, 1000.000000000000000 ) ;
#10139 = ORIENTED_EDGE ( 'NONE', *, *, #10175, .F. ) ;
#10140 = DIRECTION ( 'NONE',  ( -0.000000000000000000, 0.000000000000000000, -1.000000000000000000 ) ) ;
#10141 = DIRECTION ( 'NONE',  ( 0.000000000000000000, 0.000000000000000000, -1.000000000000000000 ) ) ;
#10142 = CARTESIAN_POINT ( 'NONE',  ( -3.522875095019672109, 2.820352903225427532, -3.598441714920591394 ) ) ;
#10143 = DIRECTION ( 'NONE',  ( -0.2873478855663453846, -0.9578262852211513190, -0.000000000000000000 ) ) ;
#10144 =( NAMED_UNIT ( * ) SI_UNIT ( $, .STERADIAN. ) SOLID_ANGLE_UNIT ( ) );
#10145 = CIRCLE ( 'NONE', #3800, 5.199999999999707079 ) ;
#10146 = EDGE_CURVE ( 'NONE', #7138, #2902, #7321, .T. ) ;
#10147 = ORIENTED_EDGE ( 'NONE', *, *, #1242, .T. ) ;
#10148 = AXIS2_PLACEMENT_3D ( 'NONE', #4295, #7535, #1773 ) ;
#10149 = DIRECTION ( 'NONE',  ( 1.000000000000000000, 0.000000000000000000, -0.000000000000000000 ) ) ;
#10150 = VERTEX_POINT ( 'NONE', #6207 ) ;
#10151 = ORIENTED_EDGE ( 'NONE', *, *, #8270, .F. ) ;
#10152 = LINE ( 'NONE', #9188, #8979 ) ;
#10153 = AXIS2_PLACEMENT_3D ( 'NONE', #7483, #10055, #11980 ) ;
#10154 = MECHANICAL_DESIGN_GEOMETRIC_PRESENTATION_REPRESENTATION (  '', ( #1675 ), #5450 ) ;
#10155 = ORIENTED_EDGE ( 'NONE', *, *, #4204, .F. ) ;
#10156 = EDGE_CURVE ( 'NONE', #12082, #6460, #10870, .T. ) ;
#10157 = CARTESIAN_POINT ( 'NONE',  ( 148.9991633467111569, 386.6211705227183870, 190.0000000000000000 ) ) ;
#10158 = AXIS2_PLACEMENT_3D ( 'NONE', #4421, #6565, #12161 ) ;
#10159 = AXIS2_PLACEMENT_3D ( 'NONE', #12840, #2722, #7225 ) ;
#10160 = DIRECTION ( 'NONE',  ( -1.000000000000000000, -0.000000000000000000, -0.000000000000000000 ) ) ;
#10161 = ORIENTED_EDGE ( 'NONE', *, *, #3391, .T. ) ;
#10162 = CARTESIAN_POINT ( 'NONE',  ( 6.445379721942638973, 2.463581311471615187, 5.110653333236676588 ) ) ;
#10163 = FACE_BOUND ( 'NONE', #5438, .T. ) ;
#10164 = CARTESIAN_POINT ( 'NONE',  ( 137.1540310085880776, 355.9707293956415697, 210.0000000000000000 ) ) ;
#10165 = CARTESIAN_POINT ( 'NONE',  ( 2.354826896168714434, -6.962563485461402024, 0.000000000000000000 ) ) ;
#10166 = FILL_AREA_STYLE ('',( #2415 ) ) ;
#10167 = EDGE_CURVE ( 'NONE', #9876, #11914, #10636, .T. ) ;
#10168 = ORIENTED_EDGE ( 'NONE', *, *, #13661, .F. ) ;
#10169 = CARTESIAN_POINT ( 'NONE',  ( 0.2484800633750021692, 4.430380094434247518, 0.3263565795980951090 ) ) ;
#10170 = ORIENTED_EDGE ( 'NONE', *, *, #9359, .T. ) ;
#10171 = CIRCLE ( 'NONE', #2142, 2.649999999999985700 ) ;
#10172 = CIRCLE ( 'NONE', #11312, 4.799999999999968736 ) ;
#10173 = EDGE_LOOP ( 'NONE', ( #4183, #9209, #436, #2966, #1738 ) ) ;
#10174 = PLANE ( 'NONE',  #4925 ) ;
#10175 = EDGE_CURVE ( 'NONE', #4296, #3186, #2846, .T. ) ;
#10176 = PRODUCT_DEFINITION_SHAPE ( 'NONE', 'NONE',  #12337 ) ;
#10177 = ADVANCED_FACE ( 'NONE', ( #648 ), #11093, .T. ) ;
#10178 = COLOUR_RGB ( '',1.000000000000000000, 0.9490196078431372140, 0.9098039215686274384 ) ;
#10179 = DIRECTION ( 'NONE',  ( 0.000000000000000000, 0.000000000000000000, -1.000000000000000000 ) ) ;
#10180 = DIRECTION ( 'NONE',  ( 0.000000000000000000, 1.000000000000000000, -1.287488025362403787E-15 ) ) ;
#10181 = EDGE_CURVE ( 'NONE', #5856, #1758, #9380, .T. ) ;
#10182 = AXIS2_PLACEMENT_3D ( 'NONE', #4615, #146, #5714 ) ;
#10183 = DIRECTION ( 'NONE',  ( -0.9578262852211513190, 0.2873478855663453846, 0.000000000000000000 ) ) ;
#10184 = CYLINDRICAL_SURFACE ( 'NONE', #1702, 4.199999999999981526 ) ;
#10185 = DIRECTION ( 'NONE',  ( 0.000000000000000000, 0.000000000000000000, -1.000000000000000000 ) ) ;
#10186 = FACE_OUTER_BOUND ( 'NONE', #2685, .T. ) ;
#10187 = ORIENTED_EDGE ( 'NONE', *, *, #5569, .T. ) ;
#10188 = FACE_OUTER_BOUND ( 'NONE', #6286, .T. ) ;
#10189 = FACE_OUTER_BOUND ( 'NONE', #1096, .T. ) ;
#10190 = APPLICATION_PROTOCOL_DEFINITION ( 'draft international standard', 'automotive_design', 1998, #10844 ) ;
#10191 = ORIENTED_EDGE ( 'NONE', *, *, #392, .F. ) ;
#10192 = DIRECTION ( 'NONE',  ( 0.2873478855663453846, 0.9578262852211513190, 0.000000000000000000 ) ) ;
#10193 = ORIENTED_EDGE ( 'NONE', *, *, #4905, .F. ) ;
#10194 = VERTEX_POINT ( 'NONE', #6050 ) ;
#10195 = AXIS2_PLACEMENT_3D ( 'NONE', #499, #12902, #12758 ) ;
#10196 =( LENGTH_UNIT ( ) NAMED_UNIT ( * ) SI_UNIT ( .MILLI., .METRE. ) );
#10197 = CARTESIAN_POINT ( 'NONE',  ( -3.249999999999996891, 5.629165124598855208, -5.592027715088710771 ) ) ;
#10198 = PLANE ( 'NONE',  #1635 ) ;
#10199 = PRODUCT_DEFINITION_FORMATION_WITH_SPECIFIED_SOURCE ( 'ANY', '', #2905, .NOT_KNOWN. ) ;
#10200 = CARTESIAN_POINT ( 'NONE',  ( 144.7991633467111683, 386.6211705227183870, -187.0000000000000568 ) ) ;
#10201 = VECTOR ( 'NONE', #6552, 1000.000000000000000 ) ;
#10202 = CARTESIAN_POINT ( 'NONE',  ( 6.095473853218073224, -3.806361898857677506, -3.407187799184166366 ) ) ;
#10203 = ORIENTED_EDGE ( 'NONE', *, *, #10687, .T. ) ;
#10204 = ADVANCED_FACE ( 'NONE', ( #5038 ), #431, .T. ) ;
#10205 = CARTESIAN_POINT ( 'NONE',  ( 33.50000000000000000, 0.000000000000000000, 2.054999999999999716 ) ) ;
#10206 = LINE ( 'NONE', #7978, #1378 ) ;
#10207 = EDGE_CURVE ( 'NONE', #4375, #14524, #9534, .T. ) ;
#10208 = CARTESIAN_POINT ( 'NONE',  ( 6.196878017913833858, 5.292377467571573568, 0.8333333333333322601 ) ) ;
#10209 = ORIENTED_EDGE ( 'NONE', *, *, #13723, .T. ) ;
#10210 = VERTEX_POINT ( 'NONE', #10554 ) ;
#10211 = DIRECTION ( 'NONE',  ( -1.000000000000000000, 0.000000000000000000, 0.000000000000000000 ) ) ;
#10212 = CARTESIAN_POINT ( 'NONE',  ( 629.0000000000000000, 166.0000000000000284, 187.5000000000000000 ) ) ;
#10213 = AXIS2_PLACEMENT_3D ( 'NONE', #10222, #12804, #2532 ) ;
#10214 = CARTESIAN_POINT ( 'NONE',  ( 630.5661054975340676, 158.1613647612965110, 211.0000000000000000 ) ) ;
#10215 = ORIENTED_EDGE ( 'NONE', *, *, #1320, .T. ) ;
#10216 = EDGE_CURVE ( 'NONE', #5721, #6493, #7305, .T. ) ;
#10217 = ORIENTED_EDGE ( 'NONE', *, *, #4590, .T. ) ;
#10218 = CARTESIAN_POINT ( 'NONE',  ( 610.1796992002056186, 189.8973840637093247, -186.7223300543793698 ) ) ;
#10219 = CARTESIAN_POINT ( 'NONE',  ( 0.000000000000000000, 0.000000000000000000, 0.000000000000000000 ) ) ;
#10220 = CARTESIAN_POINT ( 'NONE',  ( 6.518095160332176619, 5.866179305614760864, -3.428454095615614408E-15 ) ) ;
#10221 = DIRECTION ( 'NONE',  ( -0.000000000000000000, -0.000000000000000000, -1.000000000000000000 ) ) ;
#10222 = CARTESIAN_POINT ( 'NONE',  ( 635.0000000000000000, 160.0000000000000284, 210.0000000000000000 ) ) ;
#10223 = ORIENTED_EDGE ( 'NONE', *, *, #671, .T. ) ;
#10224 = LINE ( 'NONE', #5570, #13665 ) ;
#10225 = ORIENTED_EDGE ( 'NONE', *, *, #2228, .T. ) ;
#10226 = ORIENTED_EDGE ( 'NONE', *, *, #13062, .F. ) ;
#10227 = CARTESIAN_POINT ( 'NONE',  ( -10.00000000000000000, 413.4403065089105667, -190.0000000000000000 ) ) ;
#10228 = VERTEX_POINT ( 'NONE', #8405 ) ;
#10229 = DIRECTION ( 'NONE',  ( 1.000000000000000000, 0.000000000000000000, 0.000000000000000000 ) ) ;
#10230 = EDGE_CURVE ( 'NONE', #264, #2797, #2891, .T. ) ;
#10231 = CARTESIAN_POINT ( 'NONE',  ( 455.5035746174796714, 294.6698471414878782, 210.0000000000000000 ) ) ;
#10232 = ORIENTED_EDGE ( 'NONE', *, *, #9620, .T. ) ;
#10233 = DIRECTION ( 'NONE',  ( -0.2873478855663503251, -0.9578262852211498757, 0.000000000000000000 ) ) ;
#10234 = CARTESIAN_POINT ( 'NONE',  ( 0.000000000000000000, 0.000000000000000000, 187.0000000000000000 ) ) ;
#10235 = CARTESIAN_POINT ( 'NONE',  ( 628.0000000000000000, 235.0000000000000284, -233.5000000000000000 ) ) ;
#10236 =( NAMED_UNIT ( * ) SI_UNIT ( $, .STERADIAN. ) SOLID_ANGLE_UNIT ( ) );
#10237 = VERTEX_POINT ( 'NONE', #7387 ) ;
#10238 = CARTESIAN_POINT ( 'NONE',  ( 6.196878017913830305, -3.367876570272812398, 4.166666666666666963 ) ) ;
#10239 = ORIENTED_EDGE ( 'NONE', *, *, #2130, .F. ) ;
#10240 = ORIENTED_EDGE ( 'NONE', *, *, #10795, .T. ) ;
#10241 = DIRECTION ( 'NONE',  ( 0.2873478855663478826, 0.9578262852211507639, 0.000000000000000000 ) ) ;
#10242 = CARTESIAN_POINT ( 'NONE',  ( -4.000000000000000000, -1.942223658245633811, -0.3516579909967644246 ) ) ;
#10243 = EDGE_CURVE ( 'NONE', #10412, #740, #3095, .T. ) ;
#10244 = DIRECTION ( 'NONE',  ( 0.000000000000000000, 0.4999999999999992784, -0.8660254037844389297 ) ) ;
#10245 = AXIS2_PLACEMENT_3D ( 'NONE', #3242, #3459, #7896 ) ;
#10246 = CARTESIAN_POINT ( 'NONE',  ( 627.5000000000000000, 160.0000000000000284, -210.0000059999999849 ) ) ;
#10247 = EDGE_CURVE ( 'NONE', #9111, #4012, #514, .T. ) ;
#10248 = CARTESIAN_POINT ( 'NONE',  ( 610.0832774997078332, 190.4835367118463125, -186.9433982284626552 ) ) ;
#10249 = CARTESIAN_POINT ( 'NONE',  ( 590.0000000000000000, 10.00000000000005507, 190.0000000000000000 ) ) ;
#10250 = DIRECTION ( 'NONE',  ( 1.000000000000000000, 0.000000000000000000, 0.000000000000000000 ) ) ;
#10251 = EDGE_CURVE ( 'NONE', #6408, #11788, #6268, .T. ) ;
#10252 = ORIENTED_EDGE ( 'NONE', *, *, #6024, .T. ) ;
#10253 = EDGE_CURVE ( 'NONE', #6883, #9996, #4659, .T. ) ;
#10254 = CARTESIAN_POINT ( 'NONE',  ( 228.5935732249376429, 306.3651924111320000, -184.8000000000004945 ) ) ;
#10255 = DIRECTION ( 'NONE',  ( 9.794481010665704304E-16, 3.264827003555234768E-15, -1.000000000000000000 ) ) ;
#10256 = CARTESIAN_POINT ( 'NONE',  ( 707.5067158355137735, 173.1315561368708131, 9.221513133484845664E-13 ) ) ;
#10257 = CONTEXT_DEPENDENT_SHAPE_REPRESENTATION ( #9052, #8404 ) ;
#10258 = EDGE_LOOP ( 'NONE', ( #12199, #5311 ) ) ;
#10260 = EDGE_CURVE ( 'NONE', #2949, #10957, #4265, .T. ) ;
#10259 = DIRECTION ( 'NONE',  ( 0.000000000000000000, 0.000000000000000000, -1.000000000000000000 ) ) ;
#10261 = EDGE_LOOP ( 'NONE', ( #13519, #6249, #4635, #5027 ) ) ;
#10262 = ORIENTED_EDGE ( 'NONE', *, *, #240, .F. ) ;
#10263 = SURFACE_STYLE_FILL_AREA ( #12551 ) ;
#10264 = CYLINDRICAL_SURFACE ( 'NONE', #5434, 4.199999999999926459 ) ;
#10265 = CARTESIAN_POINT ( 'NONE',  ( -6.746558653883096390, -3.895127454921857524, -6.526045885145573600 ) ) ;
#10266 = PLANE ( 'NONE',  #5213 ) ;
#10267 = CARTESIAN_POINT ( 'NONE',  ( 610.0000000000000000, 0.000000000000000000, -190.0000000000000000 ) ) ;
#10268 = ORIENTED_EDGE ( 'NONE', *, *, #8629, .T. ) ;
#10269 = EDGE_CURVE ( 'NONE', #1030, #13812, #12264, .T. ) ;
#10270 = EDGE_CURVE ( 'NONE', #4166, #8096, #1018, .T. ) ;
#10271 = CARTESIAN_POINT ( 'NONE',  ( -4.000000000000000000, -2.309401076758512694, -3.433295621305382461 ) ) ;
#10272 = LINE ( 'NONE', #132, #11272 ) ;
#10273 = FILL_AREA_STYLE ('',( #975 ) ) ;
#10275 = EDGE_CURVE ( 'NONE', #7285, #13752, #11058, .T. ) ;
#10274 = DIRECTION ( 'NONE',  ( -0.000000000000000000, -0.000000000000000000, 1.000000000000000000 ) ) ;
#10276 = ORIENTED_EDGE ( 'NONE', *, *, #9982, .T. ) ;
#10277 = ORIENTED_EDGE ( 'NONE', *, *, #14382, .F. ) ;
#10278 = CARTESIAN_POINT ( 'NONE',  ( 636.9631091326946262, 152.6952049249875927, 210.0000119999999981 ) ) ;
#10279 = CARTESIAN_POINT ( 'NONE',  ( 716.7018481736364492, 193.3416907550361543, -182.8000000000001535 ) ) ;
#10280 = CARTESIAN_POINT ( 'NONE',  ( 610.0000000000000000, 10.00000000000005507, 190.0000000000000000 ) ) ;
#10281 = FACE_BOUND ( 'NONE', #13793, .T. ) ;
#10282 = ORIENTED_EDGE ( 'NONE', *, *, #4729, .T. ) ;
#10283 = ORIENTED_EDGE ( 'NONE', *, *, #1976, .F. ) ;
#10284 = CARTESIAN_POINT ( 'NONE',  ( -1.604619215278546562E-14, -7.505553499465138501, -0.8000000000000003775 ) ) ;
#10285 = DIRECTION ( 'NONE',  ( 1.000000000000000000, 0.000000000000000000, 0.000000000000000000 ) ) ;
#10286 = DIRECTION ( 'NONE',  ( 1.000000000000000000, 0.000000000000000000, 0.000000000000000000 ) ) ;
#10287 = CARTESIAN_POINT ( 'NONE',  ( 642.0000000000000000, 153.0000000000000284, -233.5000000000000000 ) ) ;
#10288 = FACE_OUTER_BOUND ( 'NONE', #7622, .T. ) ;
#10289 =( NAMED_UNIT ( * ) SI_UNIT ( $, .STERADIAN. ) SOLID_ANGLE_UNIT ( ) );
#10290 = ORIENTED_EDGE ( 'NONE', *, *, #8876, .F. ) ;
#10291 = DIRECTION ( 'NONE',  ( -0.000000000000000000, -0.000000000000000000, -1.000000000000000000 ) ) ;
#10292 = VERTEX_POINT ( 'NONE', #3026 ) ;
#10293 = VERTEX_POINT ( 'NONE', #8920 ) ;
#10294 = DIRECTION ( 'NONE',  ( 0.000000000000000000, 0.000000000000000000, -1.000000000000000000 ) ) ;
#10295 = LINE ( 'NONE', #161, #7552 ) ;
#10296 = DIRECTION ( 'NONE',  ( 1.000000000000000000, 0.000000000000000000, 0.000000000000000000 ) ) ;
#10297 = VERTEX_POINT ( 'NONE', #10025 ) ;
#10298 = LINE ( 'NONE', #165, #3832 ) ;
#10299 = CARTESIAN_POINT ( 'NONE',  ( 629.7500000000000000, 160.0000000000000284, 190.0000000000000284 ) ) ;
#10300 = CARTESIAN_POINT ( 'NONE',  ( -2.688402820137703930, -5.953403407568491623, -0.01956314070068837160 ) ) ;
#10301 = DIRECTION ( 'NONE',  ( -0.000000000000000000, -0.000000000000000000, 1.000000000000000000 ) ) ;
#10302 = PRESENTATION_STYLE_ASSIGNMENT (( #9059 ) ) ;
#10304 = ORIENTED_EDGE ( 'NONE', *, *, #1011, .T. ) ;
#10303 = B_SPLINE_CURVE_WITH_KNOTS ( 'NONE', 3,
 ( #5958, #2704, #4857, #13932, #7204, #7050, #2771, #3827 ),
 .UNSPECIFIED., .F., .F.,
 ( 4, 2, 2, 4 ),
 ( 0.000000000000000000, 0.001493104274552341888, 0.002986208549104682908, 0.005972417098209365817 ),
 .UNSPECIFIED. ) ;
#10305 = CIRCLE ( 'NONE', #3949, 4.000000000000000000 ) ;
#10306 = CARTESIAN_POINT ( 'NONE',  ( 2.059999999999998721, 0.000000000000000000, -0.3080913168122742518 ) ) ;
#10307 = AXIS2_PLACEMENT_3D ( 'NONE', #11265, #1075, #8986 ) ;
#10308 = ORIENTED_EDGE ( 'NONE', *, *, #4852, .F. ) ;
#10309 = ADVANCED_FACE ( 'NONE', ( #7524 ), #12229, .F. ) ;
#10310 = ORIENTED_EDGE ( 'NONE', *, *, #2953, .T. ) ;
#10311 = CARTESIAN_POINT ( 'NONE',  ( 5.727634848075544127, -4.575561887445499742, -6.326622577869666308 ) ) ;
#10312 = CARTESIAN_POINT ( 'NONE',  ( -4.000000000000000000, -1.560351142792950618, -0.2242961665059814425 ) ) ;
#10313 = FACE_OUTER_BOUND ( 'NONE', #9744, .T. ) ;
#10314 = AXIS2_PLACEMENT_3D ( 'NONE', #5220, #7490, #6608 ) ;
#10315 = ORIENTED_EDGE ( 'NONE', *, *, #6926, .F. ) ;
#10316 = LINE ( 'NONE', #265, #9221 ) ;
#10317 = CARTESIAN_POINT ( 'NONE',  ( 6.500000000000000000, 3.752776749732563921, -8.000000000000000000 ) ) ;
#10318 = FACE_OUTER_BOUND ( 'NONE', #6824, .T. ) ;
#10319 = CARTESIAN_POINT ( 'NONE',  ( 3.500000000000000000, -2.309401076758502480, -4.000000000000000000 ) ) ;
#10320 = ORIENTED_EDGE ( 'NONE', *, *, #4263, .T. ) ;
#10321 = CARTESIAN_POINT ( 'NONE',  ( 0.000000000000000000, 0.000000000000000000, 0.000000000000000000 ) ) ;
#10322 = DIRECTION ( 'NONE',  ( 0.000000000000000000, 0.000000000000000000, 1.000000000000000000 ) ) ;
#10323 = CARTESIAN_POINT ( 'NONE',  ( 6.534224484704352243, 2.950930484791558950, -5.111161529262918890 ) ) ;
#10324 = ORIENTED_EDGE ( 'NONE', *, *, #4276, .T. ) ;
#10325 = EDGE_CURVE ( 'NONE', #8153, #2291, #6623, .T. ) ;
#10326 = AXIS2_PLACEMENT_3D ( 'NONE', #7161, #6043, #198 ) ;
#10327 = CARTESIAN_POINT ( 'NONE',  ( 707.5067158355132051, 162.6912496279605307, 177.6000000000001648 ) ) ;
#10328 = CIRCLE ( 'NONE', #9385, 5.000000000000004441 ) ;
#10329 = VERTEX_POINT ( 'NONE', #4287 ) ;
#10330 = ORIENTED_EDGE ( 'NONE', *, *, #12621, .F. ) ;
#10331 = FACE_OUTER_BOUND ( 'NONE', #12323, .T. ) ;
#10332 = DIRECTION ( 'NONE',  ( 0.000000000000000000, 0.000000000000000000, -1.000000000000000000 ) ) ;
#10333 = EDGE_CURVE ( 'NONE', #12986, #2721, #14314, .T. ) ;
#10334 = CARTESIAN_POINT ( 'NONE',  ( 723.8855453127956707, 217.2873478855664757, 177.5999999999999375 ) ) ;
#10335 = CIRCLE ( 'NONE', #7026, 7.500000000000000000 ) ;
#10336 = CIRCLE ( 'NONE', #11735, 2.100000000000000089 ) ;
#10337 = UNCERTAINTY_MEASURE_WITH_UNIT (LENGTH_MEASURE( 1.000000000000000082E-05 ), #8018, 'distance_accuracy_value', 'NONE');
#10338 = DIRECTION ( 'NONE',  ( 0.000000000000000000, 0.000000000000000000, -1.000000000000000000 ) ) ;
#10339 = ORIENTED_EDGE ( 'NONE', *, *, #3606, .T. ) ;
#10340 = DIRECTION ( 'NONE',  ( 0.8660254037844379305, 0.5000000000000013323, 0.000000000000000000 ) ) ;
#10341 = FACE_BOUND ( 'NONE', #12618, .T. ) ;
#10342 = DIRECTION ( 'NONE',  ( 0.000000000000000000, 0.000000000000000000, 1.000000000000000000 ) ) ;
#10343 = EDGE_CURVE ( 'NONE', #1758, #6705, #9882, .T. ) ;
#10344 = VECTOR ( 'NONE', #4649, 1000.000000000000000 ) ;
#10345 = CYLINDRICAL_SURFACE ( 'NONE', #8492, 2.500000000000000444 ) ;
#10346 = ORIENTED_EDGE ( 'NONE', *, *, #5951, .T. ) ;
#10347 = VERTEX_POINT ( 'NONE', #1919 ) ;
#10348 = CARTESIAN_POINT ( 'NONE',  ( 634.0182522957532001, 152.5000000000000000, 210.0000120000000265 ) ) ;
#10349 = PLANE ( 'NONE',  #10846 ) ;
#10350 = CIRCLE ( 'NONE', #12219, 2.649999999999985700 ) ;
#10351 = AXIS2_PLACEMENT_3D ( 'NONE', #11943, #13142, #2896 ) ;
#10352 = ADVANCED_FACE ( 'NONE', ( #3320 ), #4140, .F. ) ;
#10353 = VECTOR ( 'NONE', #394, 1000.000000000000114 ) ;
#10354 = ORIENTED_EDGE ( 'NONE', *, *, #10275, .F. ) ;
#10355 = EDGE_CURVE ( 'NONE', #8233, #5493, #7824, .T. ) ;
#10356 = VERTEX_POINT ( 'NONE', #9964 ) ;
#10357 = DIRECTION ( 'NONE',  ( 1.000000000000000000, 0.000000000000000000, 0.000000000000000000 ) ) ;
#10358 = PLANE ( 'NONE',  #4017 ) ;
#10359 = VECTOR ( 'NONE', #1483, 1000.000000000000000 ) ;
#10360 = AXIS2_PLACEMENT_3D ( 'NONE', #1145, #26, #6835 ) ;
#10361 = CARTESIAN_POINT ( 'NONE',  ( 2.500000000000000000, 1.178949249685212974, -2.042000000000001148 ) ) ;
#10362 = CARTESIAN_POINT ( 'NONE',  ( 9.498873539028489220E-16, -10.00000000000000000, -210.0000000000000000 ) ) ;
#10363 = CARTESIAN_POINT ( 'NONE',  ( 497.0347780250708638, -149.1104334075212421, -189.9999999999986358 ) ) ;
#10364 = APPLICATION_CONTEXT ( 'automotive_design' ) ;
#10365 = ORIENTED_EDGE ( 'NONE', *, *, #698, .T. ) ;
#10366 = CARTESIAN_POINT ( 'NONE',  ( -0.1750025118121544265, -4.719839900820635314, -3.469254087858253399 ) ) ;
#10367 = VERTEX_POINT ( 'NONE', #7609 ) ;
#10368 = ORIENTED_EDGE ( 'NONE', *, *, #8258, .F. ) ;
#10369 = DIRECTION ( 'NONE',  ( -0.000000000000000000, -0.000000000000000000, 1.000000000000000000 ) ) ;
#10370 = AXIS2_PLACEMENT_3D ( 'NONE', #10750, #5234, #5149 ) ;
#10371 = VECTOR ( 'NONE', #7928, 1000.000000000000000 ) ;
#10372 = LINE ( 'NONE', #8083, #13681 ) ;
#10373 = DIRECTION ( 'NONE',  ( -1.000000000000000000, -2.312964634635740689E-15, 0.000000000000000000 ) ) ;
#10374 = PRODUCT_RELATED_PRODUCT_CATEGORY ( 'part', '', ( #5136 ) ) ;
#10375 = AXIS2_PLACEMENT_3D ( 'NONE', #11650, #1546, #7005 ) ;
#10376 = ORIENTED_EDGE ( 'NONE', *, *, #6399, .F. ) ;
#10377 = CARTESIAN_POINT ( 'NONE',  ( 2.500000000000000000, -1.178949249685218748, -2.041999999999998039 ) ) ;
#10378 = DIRECTION ( 'NONE',  ( 0.2873478855663453846, 0.9578262852211513190, 0.000000000000000000 ) ) ;
#10379 = CIRCLE ( 'NONE', #8253, 2.649999999999985700 ) ;
#10380 = CARTESIAN_POINT ( 'NONE',  ( -2.133938722758560669, -6.273523403446323421, -0.09463688534107154993 ) ) ;
#10381 = FACE_OUTER_BOUND ( 'NONE', #10475, .T. ) ;
#10382 = SHAPE_REPRESENTATION_RELATIONSHIP ( 'NONE' , 'NONE' ,  #5290, #1061 ) ;
#10383 = ORIENTED_EDGE ( 'NONE', *, *, #10701, .F. ) ;
#10384 = VECTOR ( 'NONE', #10955, 1000.000000000000000 ) ;
#10385 = EDGE_CURVE ( 'NONE', #344, #9543, #11792, .T. ) ;
#10386 = AXIS2_PLACEMENT_3D ( 'NONE', #3540, #5891, #6775 ) ;
#10387 = CARTESIAN_POINT ( 'NONE',  ( -10.00000000000000000, 413.4403065089105667, 187.0000000000000000 ) ) ;
#10388 = ORIENTED_EDGE ( 'NONE', *, *, #3755, .F. ) ;
#10389 = EDGE_CURVE ( 'NONE', #11414, #12665, #2047, .T. ) ;
#10390 = ORIENTED_EDGE ( 'NONE', *, *, #2922, .T. ) ;
#10392 = DIRECTION ( 'NONE',  ( 0.9578262852211489875, -0.2873478855663534892, 0.000000000000000000 ) ) ;
#10391 = AXIS2_PLACEMENT_3D ( 'NONE', #11000, #8648, #5614 ) ;
#10393 = AXIS2_PLACEMENT_3D ( 'NONE', #1064, #9860, #8609 ) ;
#10394 = CARTESIAN_POINT ( 'NONE',  ( 641.0062790085321467, 155.3995367091426658, -210.0000000000000000 ) ) ;
#10396 = VECTOR ( 'NONE', #6925, 1000.000000000000000 ) ;
#10395 = CARTESIAN_POINT ( 'NONE',  ( 152.8304684875957378, 364.5911659626319192, -210.0000000000000000 ) ) ;
#10397 = ORIENTED_EDGE ( 'NONE', *, *, #3489, .T. ) ;
#10398 = CARTESIAN_POINT ( 'NONE',  ( 610.8620436566991430, 230.3137853645740449, 190.0000000000000000 ) ) ;
#10399 = EDGE_CURVE ( 'NONE', #13395, #3660, #865, .T. ) ;
#10400 = FACE_OUTER_BOUND ( 'NONE', #3206, .T. ) ;
#10401 = FACE_BOUND ( 'NONE', #9257, .T. ) ;
#10402 = AXIS2_PLACEMENT_3D ( 'NONE', #1072, #12365, #3299 ) ;
#10403 = CARTESIAN_POINT ( 'NONE',  ( 0.4465819873849480870, -2.886751345948518566, -5.000000000000000000 ) ) ;
#10404 = VERTEX_POINT ( 'NONE', #8849 ) ;
#10405 = DIRECTION ( 'NONE',  ( 1.000000000000000000, 0.000000000000000000, -0.000000000000000000 ) ) ;
#10406 = CARTESIAN_POINT ( 'NONE',  ( -8.505790995054884007, 418.4210031920614483, 187.0000000000000000 ) ) ;
#10407 = CONTEXT_DEPENDENT_SHAPE_REPRESENTATION ( #5096, #13966 ) ;
#10408 = EDGE_LOOP ( 'NONE', ( #14161, #143, #571, #3050 ) ) ;
#10409 = VECTOR ( 'NONE', #922, 1000.000000000000114 ) ;
#10410 = DIRECTION ( 'NONE',  ( -1.000000000000000000, 0.000000000000000000, 0.000000000000000000 ) ) ;
#10411 =( GEOMETRIC_REPRESENTATION_CONTEXT ( 3 ) GLOBAL_UNCERTAINTY_ASSIGNED_CONTEXT ( ( #284 ) ) GLOBAL_UNIT_ASSIGNED_CONTEXT ( ( #8450, #3213, #911 ) ) REPRESENTATION_CONTEXT ( 'NONE', 'WORKASPACE' ) );
#10412 = VERTEX_POINT ( 'NONE', #14391 ) ;
#10413 = EDGE_LOOP ( 'NONE', ( #8296, #12515, #1624, #8634 ) ) ;
#10414 = DIRECTION ( 'NONE',  ( 0.000000000000000000, 0.000000000000000000, 1.000000000000000000 ) ) ;
#10415 = FACE_OUTER_BOUND ( 'NONE', #2641, .T. ) ;
#10416 = DIRECTION ( 'NONE',  ( 0.000000000000000000, 0.000000000000000000, 1.000000000000000000 ) ) ;
#10417 = AXIS2_PLACEMENT_3D ( 'NONE', #9569, #10676, #550 ) ;
#10418 = EDGE_CURVE ( 'NONE', #5518, #1138, #6871, .T. ) ;
#10419 = CARTESIAN_POINT ( 'NONE',  ( 0.1597025669806076964, 1.557591170363302080, 3.999999999999993339 ) ) ;
#10420 = LINE ( 'NONE', #12919, #10498 ) ;
#10421 = ORIENTED_EDGE ( 'NONE', *, *, #7406, .F. ) ;
#10422 = DIRECTION ( 'NONE',  ( -1.000000000000000000, 0.000000000000000000, 0.000000000000000000 ) ) ;
#10423 = CARTESIAN_POINT ( 'NONE',  ( -1.654252653721913102, -3.663718938583024443, -0.01223254789874440342 ) ) ;
#10424 = CARTESIAN_POINT ( 'NONE',  ( 0.000000000000000000, 0.000000000000000000, 0.000000000000000000 ) ) ;
#10425 = CARTESIAN_POINT ( 'NONE',  ( 6.436591462021366006, 2.894509378375946351, 5.013437306331752552 ) ) ;
#10426 = ORIENTED_EDGE ( 'NONE', *, *, #7723, .T. ) ;
#10427 = ORIENTED_EDGE ( 'NONE', *, *, #7998, .F. ) ;
#10428 = DIRECTION ( 'NONE',  ( 0.000000000000000000, 0.000000000000000000, -1.000000000000000000 ) ) ;
#10429 = CARTESIAN_POINT ( 'NONE',  ( 139.8040310085880833, 355.9707293956415697, 190.0000000000000000 ) ) ;
#10430 =( GEOMETRIC_REPRESENTATION_CONTEXT ( 3 ) GLOBAL_UNCERTAINTY_ASSIGNED_CONTEXT ( ( #6208 ) ) GLOBAL_UNIT_ASSIGNED_CONTEXT ( ( #1711, #13077, #9602 ) ) REPRESENTATION_CONTEXT ( 'NONE', 'WORKASPACE' ) );
#10431 = CARTESIAN_POINT ( 'NONE',  ( 139.8040310085880833, 355.9707293956415697, -190.0000000000000000 ) ) ;
#10432 = AXIS2_PLACEMENT_3D ( 'NONE', #1977, #927, #5451 ) ;
#10433 = EDGE_CURVE ( 'NONE', #6145, #5965, #10171, .T. ) ;
#10434 = ORIENTED_EDGE ( 'NONE', *, *, #3217, .T. ) ;
#10435 = CIRCLE ( 'NONE', #9973, 2.199999999999984635 ) ;
#10436 = VERTEX_POINT ( 'NONE', #6644 ) ;
#10437 = DIRECTION ( 'NONE',  ( -1.000000000000000000, 0.000000000000000000, 0.000000000000000000 ) ) ;
#10438 = LINE ( 'NONE', #7032, #1660 ) ;
#10439 = EDGE_CURVE ( 'NONE', #3223, #11084, #5924, .T. ) ;
#10440 = DIRECTION ( 'NONE',  ( 0.000000000000000000, -1.287488025362403787E-15, -1.000000000000000000 ) ) ;
#10441 = DIRECTION ( 'NONE',  ( 1.000000000000000000, 0.000000000000000000, 0.000000000000000000 ) ) ;
#10442 =( NAMED_UNIT ( * ) SI_UNIT ( $, .STERADIAN. ) SOLID_ANGLE_UNIT ( ) );
#10443 = EDGE_CURVE ( 'NONE', #8680, #6917, #4, .T. ) ;
#10444 = ORIENTED_EDGE ( 'NONE', *, *, #10056, .T. ) ;
#10445 = ADVANCED_FACE ( 'NONE', ( #12379, #6989, #13504 ), #14609, .T. ) ;
#10446 = CARTESIAN_POINT ( 'NONE',  ( 2.500000000000000000, -1.768423874527825568, -1.020999999999998575 ) ) ;
#10447 = VERTEX_POINT ( 'NONE', #5811 ) ;
#10448 = VERTEX_POINT ( 'NONE', #5596 ) ;
#10449 = CONICAL_SURFACE ( 'NONE', #1486, 4.000000000000000000, 1.047197551196600296 ) ;
#10450 = CARTESIAN_POINT ( 'NONE',  ( 708.1388811837592812, 164.7984674554459446, 150.0000000000013358 ) ) ;
#10452 = CLOSED_SHELL ( 'NONE', ( #12159, #871, #11952, #3938, #12289, #9734, #2404, #2868, #5574, #594, #11689, #3898, #12750, #5017, #2460, #5676, #1484, #3479, #8148, #8150, #5155, #11990, #4601, #10019, #7369, #6694, #13583, #4998, #3330, #14064, #12426, #11037, #7313, #6947, #10707, #3041, #11175, #4664, #7643, #4033, #7510, #5387, #5793, #6942, #8682, #1872, #8598, #13079, #1066, #10495, #2344, #14410, #9652, #13772, #819, #8031, #2503, #10889, #6561, #3659, #7987, #11780, #13214, #4806, #2341, #14310, #10309, #12594, #7597, #8896, #4866, #13371, #6478 ) ) ;
#10451 = EDGE_CURVE ( 'NONE', #7620, #8076, #11277, .T. ) ;
#10453 = CYLINDRICAL_SURFACE ( 'NONE', #7084, 0.7500000000000000000 ) ;
#10454 = B_SPLINE_CURVE_WITH_KNOTS ( 'NONE', 3,
 ( #13401, #5364, #1972, #3297, #3161, #6482 ),
 .UNSPECIFIED., .F., .F.,
 ( 4, 2, 4 ),
 ( 0.005339748439308727480, 0.006800846765732537422, 0.008261945092156346496 ),
 .UNSPECIFIED. ) ;
#10455 = LINE ( 'NONE', #4850, #4184 ) ;
#10456 = ORIENTED_EDGE ( 'NONE', *, *, #11956, .F. ) ;
#10457 = DIRECTION ( 'NONE',  ( 0.9578262852211507639, -0.2873478855663477716, 0.000000000000000000 ) ) ;
#10458 = CARTESIAN_POINT ( 'NONE',  ( 43.50000000000000711, 0.000000000000000000, 0.000000000000000000 ) ) ;
#10459 = DIRECTION ( 'NONE',  ( 1.000000000000000000, 0.000000000000000000, -0.000000000000000000 ) ) ;
#10460 = EDGE_LOOP ( 'NONE', ( #5977, #6740, #3901, #11973 ) ) ;
#10461 = EDGE_CURVE ( 'NONE', #4023, #10210, #4504, .T. ) ;
#10462 = EDGE_CURVE ( 'NONE', #2880, #238, #5455, .T. ) ;
#10463 = LINE ( 'NONE', #14012, #6827 ) ;
#10464 = ORIENTED_EDGE ( 'NONE', *, *, #9906, .T. ) ;
#10465 = ORIENTED_EDGE ( 'NONE', *, *, #2118, .F. ) ;
#10466 = PLANE ( 'NONE',  #14347 ) ;
#10467 = FACE_OUTER_BOUND ( 'NONE', #9842, .T. ) ;
#10468 = CARTESIAN_POINT ( 'NONE',  ( 635.0000000000000000, 235.0000000000000284, -263.5000000000000000 ) ) ;
#10469 = ADVANCED_FACE ( 'NONE', ( #1162 ), #1314, .T. ) ;
#10470 = VERTEX_POINT ( 'NONE', #10246 ) ;
#10471 = CARTESIAN_POINT ( 'NONE',  ( 609.8556724072889210, 189.7221213180926611, 189.8938770989753095 ) ) ;
#10472 = PLANE ( 'NONE',  #13017 ) ;
#10473 = DIRECTION ( 'NONE',  ( -0.9578262852211513190, 0.2873478855663453846, 8.575812866481462478E-17 ) ) ;
#10474 = DIRECTION ( 'NONE',  ( 0.000000000000000000, -1.000000000000000000, 1.287488025362403787E-15 ) ) ;
#10475 = EDGE_LOOP ( 'NONE', ( #1757, #4536, #13475, #4911, #4065 ) ) ;
#10476 = CARTESIAN_POINT ( 'NONE',  ( -1.399999999999999689, 0.000000000000000000, 0.000000000000000000 ) ) ;
#10477 = PLANE ( 'NONE',  #1346 ) ;
#10478 = VERTEX_POINT ( 'NONE', #11422 ) ;
#10479 = DIRECTION ( 'NONE',  ( -1.000000000000000000, -6.938893903907222067E-15, 0.000000000000000000 ) ) ;
#10480 = VERTEX_POINT ( 'NONE', #6854 ) ;
#10481 = VERTEX_POINT ( 'NONE', #9000 ) ;
#10482 = DIRECTION ( 'NONE',  ( 0.000000000000000000, 0.000000000000000000, 1.000000000000000000 ) ) ;
#10483 = CARTESIAN_POINT ( 'NONE',  ( 4.000000000000000000, 2.309401076758515803, -0.4999999999999995559 ) ) ;
#10484 = CARTESIAN_POINT ( 'NONE',  ( 1.400000000000000133, 0.000000000000000000, 0.000000000000000000 ) ) ;
#10485 = LINE ( 'NONE', #2808, #6773 ) ;
#10486 = ORIENTED_EDGE ( 'NONE', *, *, #4324, .F. ) ;
#10487 = DIRECTION ( 'NONE',  ( 0.000000000000000000, 0.000000000000000000, 1.000000000000000000 ) ) ;
#10488 = FACE_BOUND ( 'NONE', #13190, .T. ) ;
#10489 = DIRECTION ( 'NONE',  ( 0.000000000000000000, 0.000000000000000000, -1.000000000000000000 ) ) ;
#10490 = CARTESIAN_POINT ( 'NONE',  ( 636.9746078850427011, 155.6249658629529620, -211.0000000000000000 ) ) ;
#10491 = ORIENTED_EDGE ( 'NONE', *, *, #5646, .F. ) ;
#10492 = ORIENTED_EDGE ( 'NONE', *, *, #4714, .T. ) ;
#10493 = CARTESIAN_POINT ( 'NONE',  ( 610.0000000000001137, 185.6790804732683853, -169.9999999999999716 ) ) ;
#10494 = DIRECTION ( 'NONE',  ( 1.000000000000000000, 0.000000000000000000, 0.000000000000000000 ) ) ;
#10495 = ADVANCED_FACE ( 'NONE', ( #13638 ), #5677, .F. ) ;
#10496 = CARTESIAN_POINT ( 'NONE',  ( 610.0000000000001137, 185.6790804732684137, -184.8000000000000682 ) ) ;
#10497 = ORIENTED_EDGE ( 'NONE', *, *, #5091, .T. ) ;
#10498 = VECTOR ( 'NONE', #13969, 1000.000000000000000 ) ;
#10499 = DIRECTION ( 'NONE',  ( -0.000000000000000000, -0.000000000000000000, 1.000000000000000000 ) ) ;
#10500 = CARTESIAN_POINT ( 'NONE',  ( 635.0000000000000000, 160.0000000000000284, 210.0000000000000000 ) ) ;
#10501 = CARTESIAN_POINT ( 'NONE',  ( 6.837824896291514243, -3.947820044545437224, -6.564402953523717166 ) ) ;
#10502 = CARTESIAN_POINT ( 'NONE',  ( 590.0000000000000000, 212.5596934910894333, 190.0000000000000000 ) ) ;
#10503 = DIRECTION ( 'NONE',  ( 0.000000000000000000, 0.000000000000000000, 1.000000000000000000 ) ) ;
#10504 = DIRECTION ( 'NONE',  ( -0.000000000000000000, -0.000000000000000000, -1.000000000000000000 ) ) ;
#10505 = FILL_AREA_STYLE ('',( #1569 ) ) ;
#10506 = EDGE_LOOP ( 'NONE', ( #4411, #11879, #1042, #2909 ) ) ;
#10507 = CARTESIAN_POINT ( 'NONE',  ( 4.175648173966055587, -2.207990556236547608, -3.469390959564065291 ) ) ;
#10508 = ORIENTED_EDGE ( 'NONE', *, *, #7972, .F. ) ;
#10509 = VERTEX_POINT ( 'NONE', #10100 ) ;
#10510 = DIRECTION ( 'NONE',  ( -0.000000000000000000, -0.000000000000000000, -1.000000000000000000 ) ) ;
#10511 = EDGE_CURVE ( 'NONE', #13545, #10480, #2631, .T. ) ;
#10512 = EDGE_CURVE ( 'NONE', #7886, #1138, #105, .T. ) ;
#10513 = LINE ( 'NONE', #14065, #8496 ) ;
#10514 = DIRECTION ( 'NONE',  ( 2.985317128751861403E-15, 6.087367539060710222E-15, -1.000000000000000000 ) ) ;
#10516 = EDGE_CURVE ( 'NONE', #12649, #299, #3456, .T. ) ;
#10515 = DIRECTION ( 'NONE',  ( 0.9578262852211515410, -0.2873478855663446074, 0.000000000000000000 ) ) ;
#10517 = VERTEX_POINT ( 'NONE', #2487 ) ;
#10518 = CARTESIAN_POINT ( 'NONE',  ( 610.0000000000000000, 227.4403065089105951, -187.0000000000000000 ) ) ;
#10519 = CARTESIAN_POINT ( 'NONE',  ( 629.0000000000000000, 154.0000000000000284, 187.5000000000000000 ) ) ;
#10520 = ADVANCED_FACE ( 'NONE', ( #4644 ), #2342, .T. ) ;
#10521 = CARTESIAN_POINT ( 'NONE',  ( -10.00000000000000000, 371.6790804732683569, -187.0000000000000000 ) ) ;
#10522 = SURFACE_STYLE_USAGE ( .BOTH. , #8311 ) ;
#10523 = ORIENTED_EDGE ( 'NONE', *, *, #4148, .F. ) ;
#10524 = CARTESIAN_POINT ( 'NONE',  ( 0.000000000000000000, 4.330127018922191873, 2.500000000000005773 ) ) ;
#10525 = VERTEX_POINT ( 'NONE', #1382 ) ;
#10526 = PLANE ( 'NONE',  #13402 ) ;
#10527 = PRODUCT_DEFINITION_SHAPE ( 'NONE', 'NONE',  #14619 ) ;
#10528 = LINE ( 'NONE', #12446, #14154 ) ;
#10529 = DIRECTION ( 'NONE',  ( 0.000000000000000000, -1.000000000000000000, -0.000000000000000000 ) ) ;
#10530 = EDGE_CURVE ( 'NONE', #4698, #10517, #10316, .T. ) ;
#10531 = ORIENTED_EDGE ( 'NONE', *, *, #4951, .T. ) ;
#10532 = CARTESIAN_POINT ( 'NONE',  ( 112.9652219749295341, 376.5507399164317803, 190.0000000000000000 ) ) ;
#10533 = AXIS2_PLACEMENT_3D ( 'NONE', #13666, #13813, #13748 ) ;
#10534 = AXIS2_PLACEMENT_3D ( 'NONE', #3027, #5320, #5174 ) ;
#10535 = ADVANCED_FACE ( 'NONE', ( #9134 ), #9218, .T. ) ;
#10536 = AXIS2_PLACEMENT_3D ( 'NONE', #9566, #2844, #11841 ) ;
#10537 = CARTESIAN_POINT ( 'NONE',  ( 0.000000000000000000, 0.000000000000000000, 3.469446951953614189E-15 ) ) ;
#10538 = DIRECTION ( 'NONE',  ( 0.000000000000000000, 0.4999999999999990008, -0.8660254037844391517 ) ) ;
#10539 = DIRECTION ( 'NONE',  ( -0.2873478855663466613, -0.9578262852211509859, -3.408579461568464883E-15 ) ) ;
#10540 = ORIENTED_EDGE ( 'NONE', *, *, #7922, .T. ) ;
#10541 = CARTESIAN_POINT ( 'NONE',  ( -4.204114297095464359, 1.660363174096617156, -3.602136431857887011 ) ) ;
#10542 = SURFACE_STYLE_USAGE ( .BOTH. , #9299 ) ;
#10543 = ORIENTED_EDGE ( 'NONE', *, *, #10516, .F. ) ;
#10544 = LINE ( 'NONE', #9302, #4992 ) ;
#10545 = EDGE_LOOP ( 'NONE', ( #8968, #6734, #9128, #12324 ) ) ;
#10546 = ORIENTED_EDGE ( 'NONE', *, *, #9273, .F. ) ;
#10547 = DIRECTION ( 'NONE',  ( 0.000000000000000000, 1.000000000000000000, -1.287488025362403787E-15 ) ) ;
#10548 = CARTESIAN_POINT ( 'NONE',  ( 229.2257385731833779, 308.4724102386176128, -177.6000000000002217 ) ) ;
#10549 = PRESENTATION_LAYER_ASSIGNMENT (  '', '', ( #13365 ) ) ;
#10551 = CARTESIAN_POINT ( 'NONE',  ( -6.663120783604507658, -3.846954578057057983, -6.460786012260014033 ) ) ;
#10550 = CIRCLE ( 'NONE', #9133, 2.499999999999999556 ) ;
#10552 = CARTESIAN_POINT ( 'NONE',  ( 4.000000000000000888, -0.8578082829538523635, -3.433262215449808696 ) ) ;
#10553 =( REPRESENTATION_RELATIONSHIP ('NONE','NONE', #2822, #12910 ) REPRESENTATION_RELATIONSHIP_WITH_TRANSFORMATION ( #14075 )SHAPE_REPRESENTATION_RELATIONSHIP( ) );
#10554 = CARTESIAN_POINT ( 'NONE',  ( -10.00000000000000000, 413.4403065089105667, 210.0000000000000000 ) ) ;
#10555 = CARTESIAN_POINT ( 'NONE',  ( -3.886530401411042201E-15, -4.821944789745366222, 1.648146632869001538 ) ) ;
#10556 = VERTEX_POINT ( 'NONE', #13794 ) ;
#10557 = AXIS2_PLACEMENT_3D ( 'NONE', #10649, #13083, #4003 ) ;
#10558 = TOROIDAL_SURFACE ( 'NONE', #14576, 7.900000000000002132, 0.5999999999999976463 ) ;
#10559 = DIRECTION ( 'NONE',  ( -1.000000000000000000, -0.000000000000000000, -0.000000000000000000 ) ) ;
#10560 = CARTESIAN_POINT ( 'NONE',  ( 610.0000000000001137, 185.6790804732683853, 169.9999999999999716 ) ) ;
#10561 = CARTESIAN_POINT ( 'NONE',  ( 635.0000000000000000, 160.0000000000000284, -240.0999999999999943 ) ) ;
#10562 = DIRECTION ( 'NONE',  ( -0.9578262852211513190, 0.2873478855663453846, 0.000000000000000000 ) ) ;
#10563 = ORIENTED_EDGE ( 'NONE', *, *, #1413, .T. ) ;
#10564 = ORIENTED_EDGE ( 'NONE', *, *, #11747, .F. ) ;
#10565 = DIRECTION ( 'NONE',  ( -0.000000000000000000, -0.000000000000000000, -1.000000000000000000 ) ) ;
#10566 = LINE ( 'NONE', #2605, #8992 ) ;
#10567 = CARTESIAN_POINT ( 'NONE',  ( 0.000000000000000000, 0.000000000000000000, 0.000000000000000000 ) ) ;
#10568 =( GEOMETRIC_REPRESENTATION_CONTEXT ( 3 ) GLOBAL_UNCERTAINTY_ASSIGNED_CONTEXT ( ( #5333 ) ) GLOBAL_UNIT_ASSIGNED_CONTEXT ( ( #4743, #1699, #424 ) ) REPRESENTATION_CONTEXT ( 'NONE', 'WORKASPACE' ) );
#10569 = VECTOR ( 'NONE', #8808, 1000.000000000000000 ) ;
#10570 = AXIS2_PLACEMENT_3D ( 'NONE', #11592, #3996, #1625 ) ;
#10571 = DIRECTION ( 'NONE',  ( -0.000000000000000000, -0.000000000000000000, -1.000000000000000000 ) ) ;
#10572 = EDGE_LOOP ( 'NONE', ( #7100, #14338, #11627, #14602 ) ) ;
#10573 = CARTESIAN_POINT ( 'NONE',  ( 3.500000000000000000, 2.309401076758508253, 3.999999999999993339 ) ) ;
#10574 = CARTESIAN_POINT ( 'NONE',  ( 701.6639754956653405, 161.3119797772417883, -177.6000000000005059 ) ) ;
#10575 = EDGE_CURVE ( 'NONE', #9444, #2622, #12310, .T. ) ;
#10576 = DIRECTION ( 'NONE',  ( 0.000000000000000000, -1.000000000000000000, 1.287488025362403787E-15 ) ) ;
#10577 = ADVANCED_FACE ( 'NONE', ( #8465 ), #2650, .F. ) ;
#10578 = LINE ( 'NONE', #2749, #6563 ) ;
#10579 = DIRECTION ( 'NONE',  ( 0.000000000000000000, 0.000000000000000000, 1.000000000000000000 ) ) ;
#10580 =( NAMED_UNIT ( * ) PLANE_ANGLE_UNIT ( ) SI_UNIT ( $, .RADIAN. ) );
#10581 = FILL_AREA_STYLE_COLOUR ( '', #5932 ) ;
#10582 = EDGE_LOOP ( 'NONE', ( #10882, #8559, #376, #3829, #11569, #91, #11269, #3117, #14006, #1013 ) ) ;
#10583 = VECTOR ( 'NONE', #12345, 1000.000000000000114 ) ;
#10584 = CARTESIAN_POINT ( 'NONE',  ( 4.236525694536557474, -2.416953475386482530, -3.751298745799839462 ) ) ;
#10585 = VERTEX_POINT ( 'NONE', #12899 ) ;
#10586 = VERTEX_POINT ( 'NONE', #12674 ) ;
#10587 = CARTESIAN_POINT ( 'NONE',  ( 702.5260191523636877, 164.1854586329052381, -149.9999999999986642 ) ) ;
#10588 = TOROIDAL_SURFACE ( 'NONE', #3759, 4.000000000000000000, 0.2500000000000000000 ) ;
#10589 = DIRECTION ( 'NONE',  ( -0.2873478855663453846, -0.9578262852211513190, -0.000000000000000000 ) ) ;
#10590 = CARTESIAN_POINT ( 'NONE',  ( 0.1996310553826625145, 1.947030205581108619, -5.000000000000000888 ) ) ;
#10591 = VECTOR ( 'NONE', #12691, 1000.000000000000000 ) ;
#10592 = FACE_OUTER_BOUND ( 'NONE', #4938, .T. ) ;
#10593 = CIRCLE ( 'NONE', #4239, 5.199999999999733724 ) ;
#10594 = ORIENTED_EDGE ( 'NONE', *, *, #6283, .F. ) ;
#10595 = DIRECTION ( 'NONE',  ( 0.000000000000000000, 0.000000000000000000, 1.000000000000000000 ) ) ;
#10596 = EDGE_CURVE ( 'NONE', #299, #604, #8164, .T. ) ;
#10597 = CARTESIAN_POINT ( 'NONE',  ( 1.500000000000001332, 0.000000000000000000, -6.750000000000000000 ) ) ;
#10598 = CARTESIAN_POINT ( 'NONE',  ( -4.175002511812151873, -2.208363329454905877, -3.469254087858246738 ) ) ;
#10599 = CARTESIAN_POINT ( 'NONE',  ( 112.9652219749295341, 376.5507399164317803, -210.0000000000000000 ) ) ;
#10600 =( NAMED_UNIT ( * ) PLANE_ANGLE_UNIT ( ) SI_UNIT ( $, .RADIAN. ) );
#10601 = ORIENTED_EDGE ( 'NONE', *, *, #4134, .F. ) ;
#10602 = MECHANICAL_DESIGN_GEOMETRIC_PRESENTATION_REPRESENTATION (  '', ( #3999 ), #12473 ) ;
#10603 = FACE_BOUND ( 'NONE', #1194, .T. ) ;
#10604 = CARTESIAN_POINT ( 'NONE',  ( 6.481779955677555272, 2.910222513313217352, -5.040653254389295235 ) ) ;
#10605 = ORIENTED_EDGE ( 'NONE', *, *, #13985, .T. ) ;
#10606 = EDGE_CURVE ( 'NONE', #5994, #12649, #4522, .T. ) ;
#10607 = CIRCLE ( 'NONE', #1164, 4.799999999999968736 ) ;
#10608 = EDGE_CURVE ( 'NONE', #7099, #14275, #10615, .T. ) ;
#10609 = DIRECTION ( 'NONE',  ( -0.000000000000000000, -0.000000000000000000, -1.000000000000000000 ) ) ;
#10610 = CARTESIAN_POINT ( 'NONE',  ( 0.000000000000000000, 0.000000000000000000, 0.000000000000000000 ) ) ;
#10611 = VECTOR ( 'NONE', #10938, 1000.000000000000000 ) ;
#10612 = VECTOR ( 'NONE', #14212, 1000.000000000000000 ) ;
#10613 = LINE ( 'NONE', #1683, #7342 ) ;
#10614 = EDGE_LOOP ( 'NONE', ( #12452, #4164, #2626, #3288, #2649 ) ) ;
#10615 = LINE ( 'NONE', #12976, #10648 ) ;
#10616 = EDGE_CURVE ( 'NONE', #2146, #1949, #22, .T. ) ;
#10617 = AXIS2_PLACEMENT_3D ( 'NONE', #1139, #6908, #4703 ) ;
#10618 = CIRCLE ( 'NONE', #6388, 2.396904916527699214 ) ;
#10619 = DIRECTION ( 'NONE',  ( -0.9578262852211498757, 0.2873478855663503251, 0.000000000000000000 ) ) ;
#10620 = CARTESIAN_POINT ( 'NONE',  ( 237.7887055630607733, 337.0156335382104089, 179.7999999999995850 ) ) ;
#10621 = CARTESIAN_POINT ( 'NONE',  ( 0.6810597143197052450, 4.461075778259290914, -3.598441714920602053 ) ) ;
#10622 = EDGE_LOOP ( 'NONE', ( #276, #2420, #6539, #2417, #10262, #12626 ) ) ;
#10623 = CARTESIAN_POINT ( 'NONE',  ( -4.000000000000000000, -0.8232339106130515116, -3.430630286862743183 ) ) ;
#10624 = VERTEX_POINT ( 'NONE', #1470 ) ;
#10625 = VECTOR ( 'NONE', #3780, 1000.000000000000000 ) ;
#10626 = EDGE_CURVE ( 'NONE', #12254, #12397, #2713, .T. ) ;
#10627 = AXIS2_PLACEMENT_3D ( 'NONE', #11304, #1110, #5623 ) ;
#10628 = EDGE_CURVE ( 'NONE', #1012, #2816, #245, .T. ) ;
#10629 = FACE_OUTER_BOUND ( 'NONE', #1973, .T. ) ;
#10630 = ORIENTED_EDGE ( 'NONE', *, *, #11246, .F. ) ;
#10631 = DIRECTION ( 'NONE',  ( 0.000000000000000000, 0.000000000000000000, 1.000000000000000000 ) ) ;
#10632 = VECTOR ( 'NONE', #4244, 1000.000000000000114 ) ;
#10633 = EDGE_CURVE ( 'NONE', #9276, #9473, #6032, .T. ) ;
#10634 = CARTESIAN_POINT ( 'NONE',  ( 5.450967621166010524, -4.358435876041012236, -0.3607371497494579193 ) ) ;
#10635 = CARTESIAN_POINT ( 'NONE',  ( 4.000000000000000000, -1.700175430507292473, -3.320327275037661785 ) ) ;
#10636 = LINE ( 'NONE', #12997, #2378 ) ;
#10637 = UNCERTAINTY_MEASURE_WITH_UNIT (LENGTH_MEASURE( 1.000000000000000082E-05 ), #390, 'distance_accuracy_value', 'NONE');
#10638 = LINE ( 'NONE', #11513, #7439 ) ;
#10639 = ORIENTED_EDGE ( 'NONE', *, *, #591, .F. ) ;
#10640 = VECTOR ( 'NONE', #4919, 1000.000000000000000 ) ;
#10641 = FACE_OUTER_BOUND ( 'NONE', #1715, .T. ) ;
#10642 = FACE_OUTER_BOUND ( 'NONE', #3542, .T. ) ;
#10643 = CARTESIAN_POINT ( 'NONE',  ( 0.000000000000000000, 0.000000000000000000, 0.000000000000000000 ) ) ;
#10644 = ADVANCED_FACE ( 'NONE', ( #9518 ), #4524, .F. ) ;
#10645 = DIRECTION ( 'NONE',  ( -1.000000000000000000, -0.000000000000000000, -0.000000000000000000 ) ) ;
#10646 = ORIENTED_EDGE ( 'NONE', *, *, #5349, .T. ) ;
#10647 = ORIENTED_EDGE ( 'NONE', *, *, #8285, .F. ) ;
#10648 = VECTOR ( 'NONE', #1752, 1000.000000000000000 ) ;
#10649 = CARTESIAN_POINT ( 'NONE',  ( 148.9991633467111569, 386.6211705227183870, -210.0000000000000000 ) ) ;
#10650 = PLANE ( 'NONE',  #12763 ) ;
#10651 = CARTESIAN_POINT ( 'NONE',  ( 707.5067158355136598, 162.6912496279593938, -177.6000000000005059 ) ) ;
#10652 =( GEOMETRIC_REPRESENTATION_CONTEXT ( 3 ) GLOBAL_UNCERTAINTY_ASSIGNED_CONTEXT ( ( #14183 ) ) GLOBAL_UNIT_ASSIGNED_CONTEXT ( ( #13240, #10731, #8657 ) ) REPRESENTATION_CONTEXT ( 'NONE', 'WORKASPACE' ) );
#10653 = FACE_OUTER_BOUND ( 'NONE', #4188, .T. ) ;
#10654 = ORIENTED_EDGE ( 'NONE', *, *, #11531, .T. ) ;
#10655 = EDGE_CURVE ( 'NONE', #9874, #2225, #789, .T. ) ;
#10656 = VECTOR ( 'NONE', #12865, 1000.000000000000000 ) ;
#10657 = DIRECTION ( 'NONE',  ( -1.000000000000000000, -0.000000000000000000, -0.000000000000000000 ) ) ;
#10658 = CARTESIAN_POINT ( 'NONE',  ( 610.0858458365329398, 190.4893660822393144, -186.9132285165672727 ) ) ;
#10659 = CARTESIAN_POINT ( 'NONE',  ( 0.03421028094652456275, -3.072372537026353712, 2.678494666091038034 ) ) ;
#10660 = EDGE_CURVE ( 'NONE', #197, #542, #3085, .T. ) ;
#10661 = DIRECTION ( 'NONE',  ( 0.000000000000000000, 0.000000000000000000, -1.000000000000000000 ) ) ;
#10662 = CARTESIAN_POINT ( 'NONE',  ( 627.2408731339806991, 284.9098836221797342, 187.0000000000001990 ) ) ;
#10663 = CARTESIAN_POINT ( 'NONE',  ( -3.861362476283256129, -2.629030857716004199, -3.671615880910374941 ) ) ;
#10664 =( NAMED_UNIT ( * ) SI_UNIT ( $, .STERADIAN. ) SOLID_ANGLE_UNIT ( ) );
#10665 = ORIENTED_EDGE ( 'NONE', *, *, #10633, .F. ) ;
#10666 = CARTESIAN_POINT ( 'NONE',  ( -20.63749999999999574, 0.000000000000000000, 0.000000000000000000 ) ) ;
#10667 = DIRECTION ( 'NONE',  ( -1.000000000000000000, 0.000000000000000000, 0.000000000000000000 ) ) ;
#10668 = EDGE_LOOP ( 'NONE', ( #7405, #580, #11872, #1551 ) ) ;
#10669 = ORIENTED_EDGE ( 'NONE', *, *, #4607, .F. ) ;
#10670 = CARTESIAN_POINT ( 'NONE',  ( -4.000000000000000888, 1.563622288139195238, -0.2253451193528307472 ) ) ;
#10671 = AXIS2_PLACEMENT_3D ( 'NONE', #1350, #10357, #227 ) ;
#10672 = LINE ( 'NONE', #8595, #6840 ) ;
#10673 = CARTESIAN_POINT ( 'NONE',  ( 0.000000000000000000, 0.000000000000000000, 0.000000000000000000 ) ) ;
#10674 = DIRECTION ( 'NONE',  ( 0.9578262852211514300, -0.2873478855663454401, 0.000000000000000000 ) ) ;
#10675 = ORIENTED_EDGE ( 'NONE', *, *, #5211, .T. ) ;
#10676 = DIRECTION ( 'NONE',  ( -0.2873478855663454401, -0.9578262852211514300, 0.000000000000000000 ) ) ;
#10677 = CARTESIAN_POINT ( 'NONE',  ( 0.000000000000000000, 0.000000000000000000, -1.000000000000000000 ) ) ;
#10678 = DIRECTION ( 'NONE',  ( -1.000000000000000000, 0.000000000000000000, 0.000000000000000000 ) ) ;
#10679 = SURFACE_STYLE_USAGE ( .BOTH. , #2640 ) ;
#10680 = CONICAL_SURFACE ( 'NONE', #3609, 4.000000000000000000, 1.047197551196600296 ) ;
#10681 = ORIENTED_EDGE ( 'NONE', *, *, #3872, .T. ) ;
#10682 = CARTESIAN_POINT ( 'NONE',  ( 610.0000000000000000, 10.00000000000005507, 190.0000000000000000 ) ) ;
#10683 = LINE ( 'NONE', #8535, #10106 ) ;
#10684 = CONTEXT_DEPENDENT_SHAPE_REPRESENTATION ( #4538, #7361 ) ;
#10685 = ORIENTED_EDGE ( 'NONE', *, *, #9087, .T. ) ;
#10686 = DIRECTION ( 'NONE',  ( -0.9578262852211499867, 0.2873478855663502696, -1.489419751501264127E-15 ) ) ;
#10687 = EDGE_CURVE ( 'NONE', #7639, #5092, #11348, .T. ) ;
#10688 = CARTESIAN_POINT ( 'NONE',  ( -5.384454397937118664, 6.702023979852544604E-16, -5.000000000000000000 ) ) ;
#10689 = CARTESIAN_POINT ( 'NONE',  ( 0.000000000000000000, 0.5192545390863916310, 0.000000000000000000 ) ) ;
#10690 = ORIENTED_EDGE ( 'NONE', *, *, #1074, .F. ) ;
#10691 = CARTESIAN_POINT ( 'NONE',  ( 610.1796992002056186, 189.8973840637093247, 186.7223300543793698 ) ) ;
#10692 = CARTESIAN_POINT ( 'NONE',  ( 1.250000000000000000, -6.429618962271402616, 0.000000000000000000 ) ) ;
#10693 = CARTESIAN_POINT ( 'NONE',  ( 6.500000000000000000, 2.227636940139130051, -0.2900584647821234374 ) ) ;
#10694 = CARTESIAN_POINT ( 'NONE',  ( 1.287237434362044075, 3.875615274277557809, -3.430618716626812059 ) ) ;
#10695 = ORIENTED_EDGE ( 'NONE', *, *, #8633, .T. ) ;
#10696 = CARTESIAN_POINT ( 'NONE',  ( -4.211405944401398038, -2.460460786169389902, -3.751298493805494072 ) ) ;
#10697 = CARTESIAN_POINT ( 'NONE',  ( 6.534838248920896930, 2.951765777552409986, -5.112608298763837489 ) ) ;
#10698 = VERTEX_POINT ( 'NONE', #4189 ) ;
#10699 = VERTEX_POINT ( 'NONE', #712 ) ;
#10700 = DIRECTION ( 'NONE',  ( 1.000000000000000000, 0.000000000000000000, 0.000000000000000000 ) ) ;
#10701 = EDGE_CURVE ( 'NONE', #11861, #10478, #7335, .T. ) ;
#10702 = LINE ( 'NONE', #11874, #4237 ) ;
#10703 = EDGE_CURVE ( 'NONE', #12841, #10293, #6627, .T. ) ;
#10704 = CARTESIAN_POINT ( 'NONE',  ( 6.390983399715590707, 2.822795037344616453, -5.110775575965826434 ) ) ;
#10705 = DIRECTION ( 'NONE',  ( -1.000000000000000000, 0.000000000000000000, 0.000000000000000000 ) ) ;
#10706 = EDGE_CURVE ( 'NONE', #11318, #11200, #13191, .T. ) ;
#10707 = ADVANCED_FACE ( 'NONE', ( #7728 ), #10832, .F. ) ;
#10708 = CARTESIAN_POINT ( 'NONE',  ( -10.00000000000003730, 371.6790804732684137, -169.9999999999999716 ) ) ;
#10709 = EDGE_LOOP ( 'NONE', ( #8950, #8942 ) ) ;
#10710 = EDGE_CURVE ( 'NONE', #1324, #2369, #6162, .T. ) ;
#10711 = CARTESIAN_POINT ( 'NONE',  ( 610.8620436566991430, 230.3137853645733912, -184.7999999999999829 ) ) ;
#10712 = CARTESIAN_POINT ( 'NONE',  ( -1.528470953320384370E-15, 3.268109542640656784, -2.339468227445699711 ) ) ;
#10713 = DIRECTION ( 'NONE',  ( 1.000000000000000000, 0.000000000000000000, 0.000000000000000000 ) ) ;
#10714 = CARTESIAN_POINT ( 'NONE',  ( 627.5000000000000000, 160.0000000000000284, -222.5000000000000000 ) ) ;
#10715 = CONICAL_SURFACE ( 'NONE', #8357, 6.500000000000000888, 0.8987552595851582282 ) ;
#10716 = ORIENTED_EDGE ( 'NONE', *, *, #5594, .T. ) ;
#10717 = VERTEX_POINT ( 'NONE', #9868 ) ;
#10718 = DIRECTION ( 'NONE',  ( -1.000000000000000000, 0.000000000000000000, 0.000000000000000000 ) ) ;
#10719 = CARTESIAN_POINT ( 'NONE',  ( -1.860589537588217608E-13, -6.201965125294058356E-13, 186.9999999999986358 ) ) ;
#10720 = CARTESIAN_POINT ( 'NONE',  ( 609.6990795428844194, 187.6157354204721912, -188.7107384553189888 ) ) ;
#10721 = CARTESIAN_POINT ( 'NONE',  ( 705.2654023280958882, 165.6605111121457981, -177.6000000000005059 ) ) ;
#10722 = EDGE_CURVE ( 'NONE', #992, #740, #3634, .T. ) ;
#10723 = ORIENTED_EDGE ( 'NONE', *, *, #12824, .T. ) ;
#10724 = EDGE_CURVE ( 'NONE', #1544, #11118, #5696, .T. ) ;
#10725 = CARTESIAN_POINT ( 'NONE',  ( 611.4942090049448780, 232.4210031920607378, -189.9999999999999716 ) ) ;
#10726 = CARTESIAN_POINT ( 'NONE',  ( 629.0000000000000000, 154.0000000000000284, 187.5000000000000000 ) ) ;
#10727 = CARTESIAN_POINT ( 'NONE',  ( 707.5067158355135462, 162.6912496279608717, 177.6000000000001648 ) ) ;
#10728 = ADVANCED_FACE ( 'NONE', ( #11921 ), #4286, .F. ) ;
#10729 = LINE ( 'NONE', #3880, #10807 ) ;
#10730 = CARTESIAN_POINT ( 'NONE',  ( 0.000000000000000000, 0.000000000000000000, 0.000000000000000000 ) ) ;
#10731 =( NAMED_UNIT ( * ) PLANE_ANGLE_UNIT ( ) SI_UNIT ( $, .RADIAN. ) );
#10732 = ORIENTED_EDGE ( 'NONE', *, *, #403, .T. ) ;
#10733 = CARTESIAN_POINT ( 'NONE',  ( 1.600000000000000089, 0.000000000000000000, 7.000000000000000000 ) ) ;
#10734 = ORIENTED_EDGE ( 'NONE', *, *, #1340, .F. ) ;
#10735 = EDGE_LOOP ( 'NONE', ( #6778, #7041, #5513, #5969 ) ) ;
#10736 = CARTESIAN_POINT ( 'NONE',  ( 3.098410542199072637, -7.060458129626440815, 0.000000000000000000 ) ) ;
#10737 = CARTESIAN_POINT ( 'NONE',  ( 635.0000000000000000, 160.0000000000000284, -207.0000000000000000 ) ) ;
#10738 = CARTESIAN_POINT ( 'NONE',  ( 628.0000000000000000, 235.0000000000000284, -233.5000000000000000 ) ) ;
#10739 = CARTESIAN_POINT ( 'NONE',  ( -5.357619327558936585E-16, 7.505553499465137612, -6.064240316920400886 ) ) ;
#10740 = ORIENTED_EDGE ( 'NONE', *, *, #8446, .F. ) ;
#10741 = CARTESIAN_POINT ( 'NONE',  ( 5.200000000000002842, 0.000000000000000000, 0.000000000000000000 ) ) ;
#10742 = CARTESIAN_POINT ( 'NONE',  ( 640.9975013179864618, 164.6091003998119788, 210.0000120000000265 ) ) ;
#10743 = CARTESIAN_POINT ( 'NONE',  ( 721.0120664571322777, 218.1493915422639986, -177.6000000000007617 ) ) ;
#10744 = FACE_OUTER_BOUND ( 'NONE', #13822, .T. ) ;
#10745 = ORIENTED_EDGE ( 'NONE', *, *, #13421, .T. ) ;
#10746 = FACE_BOUND ( 'NONE', #74, .T. ) ;
#10747 = CARTESIAN_POINT ( 'NONE',  ( 6.527192678185238073, 2.941622124011387562, -5.095038975456095187 ) ) ;
#10748 = ORIENTED_EDGE ( 'NONE', *, *, #218, .T. ) ;
#10749 = DIRECTION ( 'NONE',  ( 0.000000000000000000, -1.000000000000000000, 3.264827003555233190E-15 ) ) ;
#10750 = CARTESIAN_POINT ( 'NONE',  ( 636.7009106935324780, 155.5114698605638637, 211.0000000000000000 ) ) ;
#10751 = LINE ( 'NONE', #627, #6639 ) ;
#10752 = ORIENTED_EDGE ( 'NONE', *, *, #2786, .T. ) ;
#10753 = DIRECTION ( 'NONE',  ( 1.000000000000000000, 0.000000000000000000, 0.000000000000000000 ) ) ;
#10754 = CARTESIAN_POINT ( 'NONE',  ( 1.399999999999999689, 0.000000000000000000, 0.000000000000000000 ) ) ;
#10755 = DIRECTION ( 'NONE',  ( -0.000000000000000000, -0.000000000000000000, 1.000000000000000000 ) ) ;
#10756 = CARTESIAN_POINT ( 'NONE',  ( -0.5276280594146446346, 4.314175951381965746, -3.320322319201721495 ) ) ;
#10757 = ADVANCED_FACE ( 'NONE', ( #4056 ), #9798, .F. ) ;
#10758 = ORIENTED_EDGE ( 'NONE', *, *, #523, .F. ) ;
#10760 = EDGE_CURVE ( 'NONE', #14449, #248, #4278, .T. ) ;
#10759 = CARTESIAN_POINT ( 'NONE',  ( -4.203934362469166963, -1.640673743454851286, -3.598432614606932756 ) ) ;
#10761 = SURFACE_SIDE_STYLE ('',( #13202 ) ) ;
#10762 = ORIENTED_EDGE ( 'NONE', *, *, #7164, .T. ) ;
#10763 = EDGE_LOOP ( 'NONE', ( #6765, #4626, #308, #768, #13560, #4492 ) ) ;
#10764 = CARTESIAN_POINT ( 'NONE',  ( -5.357619327558936585E-16, 7.505553499465137612, -8.000000000000000000 ) ) ;
#10765 = CARTESIAN_POINT ( 'NONE',  ( -3.379472811782913559E-16, -7.505553499465146494, -6.177805531629065428 ) ) ;
#10766 = CARTESIAN_POINT ( 'NONE',  ( 641.5487773412237402, 163.7885571598201579, -209.9999999999999432 ) ) ;
#10767 = AXIS2_PLACEMENT_3D ( 'NONE', #10521, #10459, #319 ) ;
#10768 = PRODUCT_DEFINITION_SHAPE ( 'NONE', 'NONE',  #14632 ) ;
#10769 = DIRECTION ( 'NONE',  ( -0.000000000000000000, -0.000000000000000000, 1.000000000000000000 ) ) ;
#10770 = UNCERTAINTY_MEASURE_WITH_UNIT (LENGTH_MEASURE( 1.000000000000000082E-05 ), #7119, 'distance_accuracy_value', 'NONE');
#10771 = DIRECTION ( 'NONE',  ( 0.000000000000000000, 0.000000000000000000, -1.000000000000000000 ) ) ;
#10772 = EDGE_CURVE ( 'NONE', #13338, #9114, #12411, .T. ) ;
#10773 = ORIENTED_EDGE ( 'NONE', *, *, #12796, .T. ) ;
#10774 = DIRECTION ( 'NONE',  ( 0.000000000000000000, 0.000000000000000000, 1.000000000000000000 ) ) ;
#10775 = DIRECTION ( 'NONE',  ( 0.9578262852211524292, -0.2873478855663418874, -0.000000000000000000 ) ) ;
#10776 = APPLICATION_PROTOCOL_DEFINITION ( 'draft international standard', 'automotive_design', 1998, #14332 ) ;
#10777 = VECTOR ( 'NONE', #11926, 1000.000000000000000 ) ;
#10778 = CARTESIAN_POINT ( 'NONE',  ( 6.534838248920897819, 2.951765777552412651, 5.112608298763836601 ) ) ;
#10779 = CIRCLE ( 'NONE', #10059, 5.249999999999976907 ) ;
#10780 = EDGE_LOOP ( 'NONE', ( #13571, #9645, #9248, #1035, #5248 ) ) ;
#10781 = VERTEX_POINT ( 'NONE', #12516 ) ;
#10782 = LINE ( 'NONE', #2817, #12671 ) ;
#10783 = CYLINDRICAL_SURFACE ( 'NONE', #14384, 4.799999999999968736 ) ;
#10784 = EDGE_CURVE ( 'NONE', #3186, #4296, #3103, .T. ) ;
#10785 = PRODUCT_DEFINITION_SHAPE ( 'NONE', 'NONE',  #13881 ) ;
#10786 = CARTESIAN_POINT ( 'NONE',  ( 6.541334219041338827, 5.921300567812616933, -0.03049376373817709943 ) ) ;
#10787 = B_SPLINE_CURVE_WITH_KNOTS ( 'NONE', 3,
 ( #5538, #9972, #11369, #3403, #13578 ),
 .UNSPECIFIED., .F., .F.,
 ( 4, 1, 4 ),
 ( 0.000000000000000000, 0.003752776749732568765, 0.007505553499465137529 ),
 .UNSPECIFIED. ) ;
#10788 = CARTESIAN_POINT ( 'NONE',  ( 635.0000000000000000, 160.0000000000000284, 215.5000000000000000 ) ) ;
#10790 = EDGE_LOOP ( 'NONE', ( #3812, #2313 ) ) ;
#10789 = PRESENTATION_LAYER_ASSIGNMENT (  '', '', ( #3247 ) ) ;
#10791 = VECTOR ( 'NONE', #10503, 1000.000000000000000 ) ;
#10792 = DIRECTION ( 'NONE',  ( -1.000000000000000000, 0.000000000000000000, 0.000000000000000000 ) ) ;
#10793 = CARTESIAN_POINT ( 'NONE',  ( -3.264624719419710521E-13, -4.796980096169328966, -3.721999068284310486 ) ) ;
#10794 = CARTESIAN_POINT ( 'NONE',  ( 590.0000000000000000, 10.00000000000005507, -190.0000000000000000 ) ) ;
#10795 = EDGE_CURVE ( 'NONE', #8217, #2701, #621, .T. ) ;
#10796 = DIRECTION ( 'NONE',  ( 0.000000000000000000, 0.000000000000000000, -1.000000000000000000 ) ) ;
#10797 = CARTESIAN_POINT ( 'NONE',  ( -3.978477517404915176, -5.573260695678958321, -6.171287963165198676 ) ) ;
#10798 = DIRECTION ( 'NONE',  ( 0.000000000000000000, 0.000000000000000000, 1.000000000000000000 ) ) ;
#10799 = ORIENTED_EDGE ( 'NONE', *, *, #7804, .T. ) ;
#10800 = DIRECTION ( 'NONE',  ( 0.000000000000000000, -0.8660254037844380415, -0.5000000000000009992 ) ) ;
#10801 = ORIENTED_EDGE ( 'NONE', *, *, #14231, .T. ) ;
#10802 = EDGE_LOOP ( 'NONE', ( #8981, #8765, #2299, #10120, #4842 ) ) ;
#10803 = FACE_OUTER_BOUND ( 'NONE', #8399, .T. ) ;
#10804 = AXIS2_PLACEMENT_3D ( 'NONE', #1985, #7819, #2197 ) ;
#10805 = EDGE_CURVE ( 'NONE', #1897, #11582, #11471, .T. ) ;
#10806 = AXIS2_PLACEMENT_3D ( 'NONE', #5276, #1944, #12117 ) ;
#10807 = VECTOR ( 'NONE', #368, 1000.000000000000000 ) ;
#10808 = EDGE_CURVE ( 'NONE', #13098, #4077, #8515, .T. ) ;
#10809 = CARTESIAN_POINT ( 'NONE',  ( 7.240873133980834986, 470.9098836221799047, -187.0000000000001990 ) ) ;
#10810 = PRODUCT_DEFINITION ( 'UNKNOWN', '', #7362, #6349 ) ;
#10811 = CARTESIAN_POINT ( 'NONE',  ( -4.078421086530219064, -3.990950201428956845, -1.000000000000000000 ) ) ;
#10812 = ORIENTED_EDGE ( 'NONE', *, *, #88, .T. ) ;
#10813 = EDGE_LOOP ( 'NONE', ( #7660, #6210, #1854 ) ) ;
#10814 = CARTESIAN_POINT ( 'NONE',  ( 10.00000000000000000, -10.00000000000000000, -190.0000000000000000 ) ) ;
#10815 = CARTESIAN_POINT ( 'NONE',  ( 635.9817477042469136, 167.5000000000000853, 210.0000120000000265 ) ) ;
#10816 = VECTOR ( 'NONE', #3969, 1000.000000000000000 ) ;
#10817 = AXIS2_PLACEMENT_3D ( 'NONE', #6572, #11067, #949 ) ;
#10818 = DIRECTION ( 'NONE',  ( -0.2873478855663466613, -0.9578262852211509859, -3.408579461568464883E-15 ) ) ;
#10819 = CARTESIAN_POINT ( 'NONE',  ( 2.500000000000000000, 2.629050547790028946E-15, 2.042000000000000259 ) ) ;
#10820 =( NAMED_UNIT ( * ) SI_UNIT ( $, .STERADIAN. ) SOLID_ANGLE_UNIT ( ) );
#10821 = ORIENTED_EDGE ( 'NONE', *, *, #9691, .F. ) ;
#10822 = DIRECTION ( 'NONE',  ( -1.000000000000000000, 0.000000000000000000, 0.000000000000000000 ) ) ;
#10823 = ITEM_DEFINED_TRANSFORMATION ( 'NONE', 'NONE', #2892,  #9440 ) ;
#10824 = ORIENTED_EDGE ( 'NONE', *, *, #9193, .F. ) ;
#10825 = AXIS2_PLACEMENT_3D ( 'NONE', #7697, #10405, #3624 ) ;
#10826 = ORIENTED_EDGE ( 'NONE', *, *, #11605, .T. ) ;
#10827 = VECTOR ( 'NONE', #2952, 1000.000000000000000 ) ;
#10828 = VECTOR ( 'NONE', #11957, 1000.000000000000114 ) ;
#10829 = CARTESIAN_POINT ( 'NONE',  ( 0.000000000000000000, -1.178949249685218748, -2.041999999999998039 ) ) ;
#10830 = LINE ( 'NONE', #2938, #11809 ) ;
#10831 = VERTEX_POINT ( 'NONE', #2410 ) ;
#10832 = PLANE ( 'NONE',  #13241 ) ;
#10833 = LINE ( 'NONE', #5238, #10841 ) ;
#10834 = AXIS2_PLACEMENT_3D ( 'NONE', #8534, #13935, #6025 ) ;
#10835 = EDGE_CURVE ( 'NONE', #8286, #5212, #1679, .T. ) ;
#10836 = FACE_OUTER_BOUND ( 'NONE', #12505, .T. ) ;
#10837 = FILL_AREA_STYLE ('',( #6333 ) ) ;
#10838 = VERTEX_POINT ( 'NONE', #92 ) ;
#10839 = VECTOR ( 'NONE', #13721, 1000.000000000000000 ) ;
#10840 = ADVANCED_FACE ( 'NONE', ( #9119 ), #9707, .T. ) ;
#10841 = VECTOR ( 'NONE', #14239, 1000.000000000000000 ) ;
#10842 = SURFACE_SIDE_STYLE ('',( #1539 ) ) ;
#10843 = ORIENTED_EDGE ( 'NONE', *, *, #6815, .T. ) ;
#10844 = APPLICATION_CONTEXT ( 'automotive_design' ) ;
#10845 = ORIENTED_EDGE ( 'NONE', *, *, #10655, .T. ) ;
#10847 = DIRECTION ( 'NONE',  ( 0.9578262852211513190, -0.2873478855663454401, -2.126837879698859960E-31 ) ) ;
#10846 = AXIS2_PLACEMENT_3D ( 'NONE', #13596, #1197, #11168 ) ;
#10848 = AXIS2_PLACEMENT_3D ( 'NONE', #8591, #14127, #12184 ) ;
#10849 = DIRECTION ( 'NONE',  ( 0.2873478855663471054, 0.9578262852211508749, -1.632680918566126195E-14 ) ) ;
#10851 = AXIS2_PLACEMENT_3D ( 'NONE', #12511, #11406, #1294 ) ;
#10850 = CARTESIAN_POINT ( 'NONE',  ( 716.7018481736364492, 193.3416907550361827, -179.8000000000001535 ) ) ;
#10852 = CIRCLE ( 'NONE', #14155, 0.2000000000000000944 ) ;
#10853 = ADVANCED_FACE ( 'NONE', ( #13554 ), #4406, .T. ) ;
#10854 = DIRECTION ( 'NONE',  ( 9.794481010665704304E-16, 3.264827003555234768E-15, -1.000000000000000000 ) ) ;
#10855 = AXIS2_PLACEMENT_3D ( 'NONE', #13438, #8050, #8933 ) ;
#10856 = DIRECTION ( 'NONE',  ( -0.9578262852211503198, 0.2873478855663487153, -1.489419751501258013E-15 ) ) ;
#10857 = ORIENTED_EDGE ( 'NONE', *, *, #2488, .F. ) ;
#10858 = AXIS2_PLACEMENT_3D ( 'NONE', #12029, #7617, #9604 ) ;
#10859 = DIRECTION ( 'NONE',  ( 0.9578262852211506528, -0.2873478855663477161, -0.000000000000000000 ) ) ;
#10860 = CARTESIAN_POINT ( 'NONE',  ( 1.500000000000001332, 6.766173565289127388E-16, 5.525000000000000355 ) ) ;
#10861 = APPLICATION_PROTOCOL_DEFINITION ( 'draft international standard', 'automotive_design', 1998, #1779 ) ;
#10862 = AXIS2_PLACEMENT_3D ( 'NONE', #7863, #7923, #12346 ) ;
#10863 = CARTESIAN_POINT ( 'NONE',  ( -0.1920286436967154065, 0.000000000000000000, 6.975000000000000533 ) ) ;
#10864 = AXIS2_PLACEMENT_3D ( 'NONE', #9702, #2124, #6647 ) ;
#10865 = ORIENTED_EDGE ( 'NONE', *, *, #14437, .F. ) ;
#10866 = EDGE_LOOP ( 'NONE', ( #5878, #12375, #6247 ) ) ;
#10867 = CARTESIAN_POINT ( 'NONE',  ( 650.0000000000000000, 145.0000000000000568, -210.0000000000000000 ) ) ;
#10868 = DIRECTION ( 'NONE',  ( 1.000000000000000000, 0.000000000000000000, 0.000000000000000000 ) ) ;
#10869 = DIRECTION ( 'NONE',  ( -3.125627884642896034E-16, 4.141456947151826978E-15, 1.000000000000000000 ) ) ;
#10870 = CIRCLE ( 'NONE', #3323, 5.525000000000000355 ) ;
#10871 = EDGE_CURVE ( 'NONE', #5524, #7989, #2154, .T. ) ;
#10872 = VECTOR ( 'NONE', #10072, 1000.000000000000000 ) ;
#10873 = CARTESIAN_POINT ( 'NONE',  ( 0.000000000000000000, 0.000000000000000000, -25.03750572909317285 ) ) ;
#10874 = TOROIDAL_SURFACE ( 'NONE', #4514, 5.384454397937118664, 0.5155456020628804703 ) ;
#10875 = ORIENTED_EDGE ( 'NONE', *, *, #11528, .F. ) ;
#10876 = CARTESIAN_POINT ( 'NONE',  ( 635.0000000000000000, 160.0000000000000284, -211.0000000000000000 ) ) ;
#10877 = CARTESIAN_POINT ( 'NONE',  ( 2.999999999999999112, 2.309401076758508253, 3.999999999999993339 ) ) ;
#10878 = ORIENTED_EDGE ( 'NONE', *, *, #1248, .T. ) ;
#10879 = DIRECTION ( 'NONE',  ( -0.000000000000000000, -0.000000000000000000, -1.000000000000000000 ) ) ;
#10880 = CARTESIAN_POINT ( 'NONE',  ( 635.0000000000000000, 160.0000000000000284, -225.5000000000000000 ) ) ;
#10881 = AXIS2_PLACEMENT_3D ( 'NONE', #6485, #5519, #13333 ) ;
#10882 = ORIENTED_EDGE ( 'NONE', *, *, #4185, .F. ) ;
#10883 = AXIS2_PLACEMENT_3D ( 'NONE', #2380, #14560, #9029 ) ;
#10884 = CARTESIAN_POINT ( 'NONE',  ( -20.63749999999999574, 0.000000000000000000, 0.000000000000000000 ) ) ;
#10885 = EDGE_LOOP ( 'NONE', ( #6910, #5602, #4227, #10630 ) ) ;
#10886 = ORIENTED_EDGE ( 'NONE', *, *, #9564, .T. ) ;
#10887 = LINE ( 'NONE', #13310, #5656 ) ;
#10888 =( GEOMETRIC_REPRESENTATION_CONTEXT ( 3 ) GLOBAL_UNCERTAINTY_ASSIGNED_CONTEXT ( ( #732 ) ) GLOBAL_UNIT_ASSIGNED_CONTEXT ( ( #9644, #2173, #4465 ) ) REPRESENTATION_CONTEXT ( 'NONE', 'WORKASPACE' ) );
#10889 = ADVANCED_FACE ( 'NONE', ( #11261 ), #1299, .T. ) ;
#10890 = LINE ( 'NONE', #4169, #2628 ) ;
#10891 = EDGE_CURVE ( 'NONE', #9509, #10781, #12528, .T. ) ;
#10892 = ORIENTED_EDGE ( 'NONE', *, *, #4207, .F. ) ;
#10893 = ORIENTED_EDGE ( 'NONE', *, *, #5055, .T. ) ;
#10894 = CARTESIAN_POINT ( 'NONE',  ( 6.204460410672268722, -3.831267809383453571, 3.364049496744554002 ) ) ;
#10895 = PLANE ( 'NONE',  #11773 ) ;
#10896 = EDGE_CURVE ( 'NONE', #6340, #14092, #14590, .T. ) ;
#10897 = AXIS2_PLACEMENT_3D ( 'NONE', #4891, #5919, #13974 ) ;
#10898 = CARTESIAN_POINT ( 'NONE',  ( 630.0000000000000000, 160.0000000000000284, -222.5000000000000000 ) ) ;
#10899 = FACE_OUTER_BOUND ( 'NONE', #3400, .T. ) ;
#10900 = EDGE_LOOP ( 'NONE', ( #12293, #7813, #5214, #3618 ) ) ;
#10901 = EDGE_CURVE ( 'NONE', #7181, #14510, #10298, .T. ) ;
#10902 = DIRECTION ( 'NONE',  ( 1.000000000000000000, 0.000000000000000000, 0.000000000000000000 ) ) ;
#10903 = DIRECTION ( 'NONE',  ( 0.000000000000000000, 0.000000000000000000, -1.000000000000000000 ) ) ;
#10904 = ORIENTED_EDGE ( 'NONE', *, *, #12485, .T. ) ;
#10905 = VECTOR ( 'NONE', #2190, 1000.000000000000227 ) ;
#10906 = FACE_OUTER_BOUND ( 'NONE', #110, .T. ) ;
#10907 = EDGE_LOOP ( 'NONE', ( #1488, #5515, #10843, #4262 ) ) ;
#10908 = AXIS2_PLACEMENT_3D ( 'NONE', #14258, #7395, #12102 ) ;
#10909 = CARTESIAN_POINT ( 'NONE',  ( 0.000000000000000000, 1.178949249685217415, 2.041999999999998483 ) ) ;
#10910 = CARTESIAN_POINT ( 'NONE',  ( 144.7991633467111399, 386.6211705227183870, -210.0000000000000000 ) ) ;
#10911 = AXIS2_PLACEMENT_3D ( 'NONE', #6022, #389, #6099 ) ;
#10912 = ORIENTED_EDGE ( 'NONE', *, *, #1917, .T. ) ;
#10913 = CARTESIAN_POINT ( 'NONE',  ( 610.3730626637085379, 189.1846890958936740, 186.1333820183295984 ) ) ;
#10914 = DIRECTION ( 'NONE',  ( 1.224646799147353207E-16, 1.000000000000000000, 0.000000000000000000 ) ) ;
#10915 = EDGE_CURVE ( 'NONE', #13614, #12303, #976, .T. ) ;
#10916 = ADVANCED_FACE ( 'NONE', ( #4482 ), #12590, .T. ) ;
#10917 = VECTOR ( 'NONE', #10499, 1000.000000000000000 ) ;
#10918 = CARTESIAN_POINT ( 'NONE',  ( 716.7018481736364492, 193.3416907550376322, 179.8000000000001535 ) ) ;
#10919 = ORIENTED_EDGE ( 'NONE', *, *, #4409, .F. ) ;
#10920 = LINE ( 'NONE', #794, #3776 ) ;
#10921 = CARTESIAN_POINT ( 'NONE',  ( -6.500000000000000000, 3.453380256388206782, -0.6809028088495794329 ) ) ;
#10922 = ORIENTED_EDGE ( 'NONE', *, *, #14497, .T. ) ;
#10923 = ORIENTED_EDGE ( 'NONE', *, *, #8891, .T. ) ;
#10924 = PLANE ( 'NONE',  #11975 ) ;
#10925 = FACE_OUTER_BOUND ( 'NONE', #12420, .T. ) ;
#10926 = B_SPLINE_CURVE_WITH_KNOTS ( 'NONE', 3,
 ( #10697, #12764, #7376, #12985, #11869, #1540, #272, #13867 ),
 .UNSPECIFIED., .F., .F.,
 ( 4, 2, 2, 4 ),
 ( 0.000000000000000000, 0.001493104274552342322, 0.002986208549104683342, 0.005972417098209364950 ),
 .UNSPECIFIED. ) ;
#10927 = CARTESIAN_POINT ( 'NONE',  ( 635.0000000000000000, 160.0000000000000284, -207.0000000000000000 ) ) ;
#10928 = DIRECTION ( 'NONE',  ( -1.000000000000000000, 0.000000000000000000, -0.000000000000000000 ) ) ;
#10929 = DIRECTION ( 'NONE',  ( 0.2873478855663453291, 0.9578262852211513190, 0.000000000000000000 ) ) ;
#10930 = ORIENTED_EDGE ( 'NONE', *, *, #11602, .F. ) ;
#10931 = CARTESIAN_POINT ( 'NONE',  ( -6.473970235329672780E-16, -4.862606272033106691, -3.745885042887442395 ) ) ;
#10932 = DIRECTION ( 'NONE',  ( -1.000000000000000000, -0.000000000000000000, -0.000000000000000000 ) ) ;
#10933 = CARTESIAN_POINT ( 'NONE',  ( 148.9991633467111569, 386.6211705227183870, -218.0000000000000000 ) ) ;
#10934 = LINE ( 'NONE', #8639, #947 ) ;
#10935 = ORIENTED_EDGE ( 'NONE', *, *, #5661, .T. ) ;
#10936 = ORIENTED_EDGE ( 'NONE', *, *, #12605, .T. ) ;
#10937 = DIRECTION ( 'NONE',  ( 0.2873478855663452736, 0.9578262852211513190, -3.491481338843133355E-15 ) ) ;
#10938 = DIRECTION ( 'NONE',  ( 0.000000000000000000, 1.000000000000000000, -0.000000000000000000 ) ) ;
#10939 = CARTESIAN_POINT ( 'NONE',  ( 6.242800618755108388, 4.918813924286816963, 1.690830708135752758 ) ) ;
#10940 = CARTESIAN_POINT ( 'NONE',  ( -8.505790995055066972, 376.6597771564184427, -187.0000000000000284 ) ) ;
#10941 = ORIENTED_EDGE ( 'NONE', *, *, #10207, .F. ) ;
#10942 = UNCERTAINTY_MEASURE_WITH_UNIT (LENGTH_MEASURE( 1.000000000000000082E-05 ), #4299, 'distance_accuracy_value', 'NONE');
#10943 = DIRECTION ( 'NONE',  ( 0.000000000000000000, -1.000000000000000000, 0.000000000000000000 ) ) ;
#10944 = EDGE_LOOP ( 'NONE', ( #8760, #11634 ) ) ;
#10945 = CARTESIAN_POINT ( 'NONE',  ( 641.0000000000000000, 154.0000000000000568, -187.5000000000000000 ) ) ;
#10946 = CARTESIAN_POINT ( 'NONE',  ( -0.5619217318086660029, -7.564468822943311466, -6.443866470201765395 ) ) ;
#10947 = LINE ( 'NONE', #601, #10569 ) ;
#10948 = ADVANCED_FACE ( 'NONE', ( #5871 ), #6757, .F. ) ;
#10949 = ORIENTED_EDGE ( 'NONE', *, *, #12706, .T. ) ;
#10950 = CARTESIAN_POINT ( 'NONE',  ( 0.03363697881402284012, -0.7786124122131168335, 3.999999999999997335 ) ) ;
#10951 = VERTEX_POINT ( 'NONE', #11552 ) ;
#10952 = EDGE_LOOP ( 'NONE', ( #12806, #3631, #10223, #6476 ) ) ;
#10953 = DIRECTION ( 'NONE',  ( -0.000000000000000000, -0.000000000000000000, 1.000000000000000000 ) ) ;
#10954 = EDGE_CURVE ( 'NONE', #3170, #8139, #5243, .T. ) ;
#10955 = DIRECTION ( 'NONE',  ( 0.000000000000000000, -1.000000000000000000, 0.000000000000000000 ) ) ;
#10956 = ORIENTED_EDGE ( 'NONE', *, *, #4501, .T. ) ;
#10957 = VERTEX_POINT ( 'NONE', #14069 ) ;
#10958 = CARTESIAN_POINT ( 'NONE',  ( 6.390820841722131718, -5.837016270311241151, -0.1100087447852492878 ) ) ;
#10959 = CARTESIAN_POINT ( 'NONE',  ( 708.1388811837590538, 164.7984674554467404, 177.5999999999999091 ) ) ;
#10960 = DIRECTION ( 'NONE',  ( -1.000000000000000000, 0.000000000000000000, -1.063400795443704616E-15 ) ) ;
#10961 = DIRECTION ( 'NONE',  ( 0.000000000000000000, 0.000000000000000000, -1.000000000000000000 ) ) ;
#10962 = EDGE_CURVE ( 'NONE', #13246, #12104, #7271, .T. ) ;
#10963 = ORIENTED_EDGE ( 'NONE', *, *, #11153, .F. ) ;
#10964 = LINE ( 'NONE', #9856, #5403 ) ;
#10965 = CONTEXT_DEPENDENT_SHAPE_REPRESENTATION ( #13774, #11010 ) ;
#10966 = ORIENTED_EDGE ( 'NONE', *, *, #13526, .F. ) ;
#10967 = PLANE ( 'NONE',  #4751 ) ;
#10968 = EDGE_CURVE ( 'NONE', #2500, #681, #3351, .T. ) ;
#10969 = VERTEX_POINT ( 'NONE', #8443 ) ;
#10970 = ADVANCED_FACE ( 'NONE', ( #2702 ), #12959, .F. ) ;
#10971 = CARTESIAN_POINT ( 'NONE',  ( 0.000000000000000000, 0.000000000000000000, 0.000000000000000000 ) ) ;
#10972 = DIRECTION ( 'NONE',  ( -0.000000000000000000, -0.000000000000000000, -1.000000000000000000 ) ) ;
#10973 = EDGE_CURVE ( 'NONE', #8255, #689, #2874, .T. ) ;
#10974 = ORIENTED_EDGE ( 'NONE', *, *, #4749, .T. ) ;
#10975 = DIRECTION ( 'NONE',  ( 0.000000000000000000, 0.000000000000000000, 1.000000000000000000 ) ) ;
#10976 = DIRECTION ( 'NONE',  ( 1.000000000000000000, 0.000000000000000000, -0.000000000000000000 ) ) ;
#10977 = CARTESIAN_POINT ( 'NONE',  ( 443.6584422793565636, 264.0194060144110608, 187.0000000000000000 ) ) ;
#10978 = ORIENTED_EDGE ( 'NONE', *, *, #4204, .T. ) ;
#10979 = DIRECTION ( 'NONE',  ( 0.000000000000000000, 0.000000000000000000, -1.000000000000000000 ) ) ;
#10980 = ORIENTED_EDGE ( 'NONE', *, *, #1602, .T. ) ;
#10981 = ORIENTED_EDGE ( 'NONE', *, *, #8516, .T. ) ;
#10982 = CARTESIAN_POINT ( 'NONE',  ( -0.2813450144774474748, -7.667988119308860817, -6.122077150241856280 ) ) ;
#10983 = EDGE_CURVE ( 'NONE', #5936, #9268, #3825, .T. ) ;
#10984 = CARTESIAN_POINT ( 'NONE',  ( 0.000000000000000000, 0.000000000000000000, -7.974599999999998801 ) ) ;
#10985 = PLANE ( 'NONE',  #7324 ) ;
#10986 = EDGE_CURVE ( 'NONE', #12480, #3563, #12227, .T. ) ;
#10987 = CARTESIAN_POINT ( 'NONE',  ( 2.500000000000000000, 2.357898499370431722, -2.818925648462311528E-15 ) ) ;
#10988 = CARTESIAN_POINT ( 'NONE',  ( 459.3348797583642522, 272.6398425814014104, 190.0000000000000000 ) ) ;
#10989 = ORIENTED_EDGE ( 'NONE', *, *, #13825, .T. ) ;
#10990 = CARTESIAN_POINT ( 'NONE',  ( 650.0000000000000000, 175.0000000000000568, -190.0000000000000000 ) ) ;
#10991 = CARTESIAN_POINT ( 'NONE',  ( 6.244889965166096069, -3.924082311521026600, -3.413878157001048574 ) ) ;
#10992 = APPLICATION_PROTOCOL_DEFINITION ( 'draft international standard', 'automotive_design', 1998, #1226 ) ;
#10993 = CARTESIAN_POINT ( 'NONE',  ( 148.9991633467111569, 386.6211705227183870, -210.0000000000000000 ) ) ;
#10994 = ORIENTED_EDGE ( 'NONE', *, *, #6106, .F. ) ;
#10995 = ORIENTED_EDGE ( 'NONE', *, *, #11684, .T. ) ;
#10996 = B_SPLINE_CURVE_WITH_KNOTS ( 'NONE', 3,
 ( #14151, #3830, #1676, #9575, #3749, #486, #7356, #12747 ),
 .UNSPECIFIED., .F., .F.,
 ( 4, 2, 2, 4 ),
 ( 2.459764730720142121E-07, 0.001920659145285718043, 0.002880865729692040113, 0.003841072314098362400 ),
 .UNSPECIFIED. ) ;
#10997 = CARTESIAN_POINT ( 'NONE',  ( 448.9584422793565750, 264.0194060144110608, 187.0000000000000000 ) ) ;
#10998 = FACE_OUTER_BOUND ( 'NONE', #8520, .T. ) ;
#10999 = CARTESIAN_POINT ( 'NONE',  ( -1.399999999999998579, 0.000000000000000000, 0.000000000000000000 ) ) ;
#11000 = CARTESIAN_POINT ( 'NONE',  ( 139.8040310085880833, 355.9707293956415697, -190.0000000000000000 ) ) ;
#11001 = ORIENTED_EDGE ( 'NONE', *, *, #4803, .F. ) ;
#11002 = PLANE ( 'NONE',  #12309 ) ;
#11003 = ORIENTED_EDGE ( 'NONE', *, *, #6345, .T. ) ;
#11004 = CIRCLE ( 'NONE', #1614, 5.199999999999760369 ) ;
#11005 = AXIS2_PLACEMENT_3D ( 'NONE', #12654, #2406, #6909 ) ;
#11006 = LINE ( 'NONE', #13159, #9633 ) ;
#11007 = CARTESIAN_POINT ( 'NONE',  ( 3.783380760145018981E-16, -7.895640089090872671, -6.564402953523720718 ) ) ;
#11008 = LINE ( 'NONE', #822, #6096 ) ;
#11009 =( NAMED_UNIT ( * ) PLANE_ANGLE_UNIT ( ) SI_UNIT ( $, .RADIAN. ) );
#11010 = PRODUCT_DEFINITION_SHAPE ( 'NONE', 'NONE',  #14644 ) ;
#11011 = VERTEX_POINT ( 'NONE', #8228 ) ;
#11012 = EDGE_CURVE ( 'NONE', #2902, #1012, #8307, .T. ) ;
#11013 = AXIS2_PLACEMENT_3D ( 'NONE', #13746, #4526, #61 ) ;
#11014 = CARTESIAN_POINT ( 'NONE',  ( 0.2486750293982080140, -1.933232340707284447, 3.999999999999998224 ) ) ;
#11015 = ORIENTED_EDGE ( 'NONE', *, *, #14296, .F. ) ;
#11016 = VERTEX_POINT ( 'NONE', #9419 ) ;
#11017 = DIRECTION ( 'NONE',  ( 0.000000000000000000, -1.000000000000000000, 0.000000000000000000 ) ) ;
#11018 = CARTESIAN_POINT ( 'NONE',  ( 4.101954839143203912, 2.368264730583012234, -3.681130640444374436 ) ) ;
#11019 = AXIS2_PLACEMENT_3D ( 'NONE', #13430, #10255, #13734 ) ;
#11020 = CARTESIAN_POINT ( 'NONE',  ( -2.000000000000006661, 3.464101615137750834, 0.000000000000000000 ) ) ;
#11021 = EDGE_LOOP ( 'NONE', ( #9927, #12183, #8170, #13934, #1259, #3887 ) ) ;
#11022 = ADVANCED_FACE ( 'NONE', ( #12738 ), #7348, .F. ) ;
#11023 = VERTEX_POINT ( 'NONE', #2768 ) ;
#11024 = CARTESIAN_POINT ( 'NONE',  ( 6.367873360227558344, 5.773502691896261751, 0.000000000000000000 ) ) ;
#11025 = CARTESIAN_POINT ( 'NONE',  ( 6.500000000000000888, 3.402385889607308922, -5.998095356498452269 ) ) ;
#11026 = CARTESIAN_POINT ( 'NONE',  ( -0.6640947660597427138, 4.471078309994878985, -3.602146406945963442 ) ) ;
#11027 = FACE_OUTER_BOUND ( 'NONE', #1955, .T. ) ;
#11028 = FACE_OUTER_BOUND ( 'NONE', #11479, .T. ) ;
#11029 = PRESENTATION_STYLE_ASSIGNMENT (( #694 ) ) ;
#11030 = VERTEX_POINT ( 'NONE', #10377 ) ;
#11031 = CIRCLE ( 'NONE', #6560, 5.525000000000000355 ) ;
#11032 = CIRCLE ( 'NONE', #7496, 4.000000000000000000 ) ;
#11033 = ORIENTED_EDGE ( 'NONE', *, *, #10530, .F. ) ;
#11034 = PLANE ( 'NONE',  #9224 ) ;
#11035 = ORIENTED_EDGE ( 'NONE', *, *, #2028, .T. ) ;
#11036 = DIRECTION ( 'NONE',  ( 0.000000000000000000, 0.000000000000000000, -1.000000000000000000 ) ) ;
#11037 = ADVANCED_FACE ( 'NONE', ( #7133 ), #6177, .T. ) ;
#11038 = CARTESIAN_POINT ( 'NONE',  ( 470.8287951810180516, 310.9528939902474463, 190.0000000000000000 ) ) ;
#11039 = AXIS2_PLACEMENT_3D ( 'NONE', #5966, #101, #3615 ) ;
#11040 = VECTOR ( 'NONE', #5412, 1000.000000000000000 ) ;
#11041 = CIRCLE ( 'NONE', #12934, 4.799999999999999822 ) ;
#11042 = ORIENTED_EDGE ( 'NONE', *, *, #9090, .T. ) ;
#11043 = DIRECTION ( 'NONE',  ( 0.000000000000000000, 0.000000000000000000, -1.000000000000000000 ) ) ;
#11044 = DIRECTION ( 'NONE',  ( -0.7071067811865474617, 8.659560562354932858E-17, -0.7071067811865474617 ) ) ;
#11045 = DIRECTION ( 'NONE',  ( 0.9578262852211514300, -0.2873478855663453846, -1.407442229263725984E-15 ) ) ;
#11046 = ORIENTED_EDGE ( 'NONE', *, *, #12503, .F. ) ;
#11047 = AXIS2_PLACEMENT_3D ( 'NONE', #14487, #4584, #11365 ) ;
#11048 =( NAMED_UNIT ( * ) PLANE_ANGLE_UNIT ( ) SI_UNIT ( $, .RADIAN. ) );
#11049 = ORIENTED_EDGE ( 'NONE', *, *, #11342, .T. ) ;
#11050 = CIRCLE ( 'NONE', #4705, 6.750000000000000000 ) ;
#11051 = AXIS2_PLACEMENT_3D ( 'NONE', #2811, #7456, #9819 ) ;
#11052 = ORIENTED_EDGE ( 'NONE', *, *, #10724, .F. ) ;
#11053 = CARTESIAN_POINT ( 'NONE',  ( 10.00000000000000000, 386.5596934910894902, -210.0000000000000000 ) ) ;
#11054 = LINE ( 'NONE', #937, #8937 ) ;
#11055 = ADVANCED_FACE ( 'NONE', ( #5075 ), #11628, .T. ) ;
#11056 = VECTOR ( 'NONE', #12070, 1000.000000000000114 ) ;
#11057 = CARTESIAN_POINT ( 'NONE',  ( 631.2114428402037447, 166.5487773412478987, -210.0000000000000000 ) ) ;
#11058 = LINE ( 'NONE', #3176, #11334 ) ;
#11059 = CIRCLE ( 'NONE', #9666, 4.199999999999926459 ) ;
#11060 = AXIS2_PLACEMENT_3D ( 'NONE', #6068, #10571, #9549 ) ;
#11061 = CARTESIAN_POINT ( 'NONE',  ( 4.424031367836657402, 4.951337798342080099, -6.056431503344841261 ) ) ;
#11062 = CARTESIAN_POINT ( 'NONE',  ( 635.0000000000000000, 160.0000000000000284, -210.0000000000000000 ) ) ;
#11063 = EDGE_CURVE ( 'NONE', #14014, #9797, #1520, .T. ) ;
#11064 = EDGE_LOOP ( 'NONE', ( #6902, #8243, #2916, #253 ) ) ;
#11065 = ADVANCED_FACE ( 'NONE', ( #12816 ), #9277, .F. ) ;
#11066 = DIRECTION ( 'NONE',  ( -1.000000000000000000, -0.000000000000000000, -0.000000000000000000 ) ) ;
#11067 = DIRECTION ( 'NONE',  ( -1.000000000000000000, -0.000000000000000000, -0.000000000000000000 ) ) ;
#11068 = AXIS2_PLACEMENT_3D ( 'NONE', #13914, #8365, #9407 ) ;
#11070 = EDGE_CURVE ( 'NONE', #3137, #7506, #8147, .T. ) ;
#11069 = DIRECTION ( 'NONE',  ( 0.000000000000000000, 0.000000000000000000, 1.000000000000000000 ) ) ;
#11071 = VERTEX_POINT ( 'NONE', #1957 ) ;
#11072 = EDGE_LOOP ( 'NONE', ( #10654, #9159, #1121, #13308 ) ) ;
#11073 = SURFACE_STYLE_FILL_AREA ( #11292 ) ;
#11074 = CARTESIAN_POINT ( 'NONE',  ( 640.0000000000000000, 160.0000000000000284, 215.5000000000000000 ) ) ;
#11075 = CIRCLE ( 'NONE', #6361, 4.200000000000009059 ) ;
#11076 = VECTOR ( 'NONE', #2747, 1000.000000000000000 ) ;
#11077 = DIRECTION ( 'NONE',  ( 1.000000000000000000, 0.000000000000000000, 0.000000000000000000 ) ) ;
#11078 = VECTOR ( 'NONE', #1559, 1000.000000000000000 ) ;
#11079 = DIRECTION ( 'NONE',  ( 9.963058866566169367E-16, 3.321019622188723517E-15, 1.000000000000000000 ) ) ;
#11080 = VECTOR ( 'NONE', #10274, 1000.000000000000000 ) ;
#11081 = ORIENTED_EDGE ( 'NONE', *, *, #8325, .T. ) ;
#11082 = UNCERTAINTY_MEASURE_WITH_UNIT (LENGTH_MEASURE( 1.000000000000000082E-05 ), #12770, 'distance_accuracy_value', 'NONE');
#11083 = CARTESIAN_POINT ( 'NONE',  ( -6.500000000000000000, -4.014037567183532218, -6.470355840301004413 ) ) ;
#11084 = VERTEX_POINT ( 'NONE', #4036 ) ;
#11085 = EDGE_CURVE ( 'NONE', #7201, #4236, #5015, .T. ) ;
#11086 = AXIS2_PLACEMENT_3D ( 'NONE', #8373, #11685, #1579 ) ;
#11087 = DIRECTION ( 'NONE',  ( 1.000000000000000000, 0.000000000000000000, 0.000000000000000000 ) ) ;
#11088 = LINE ( 'NONE', #4811, #7279 ) ;
#11089 = LINE ( 'NONE', #4798, #7752 ) ;
#11090 = FACE_OUTER_BOUND ( 'NONE', #12785, .T. ) ;
#11091 = VERTEX_POINT ( 'NONE', #2927 ) ;
#11092 = EDGE_LOOP ( 'NONE', ( #13958, #33, #12584, #10732, #5974, #11403, #7132, #7692 ) ) ;
#11093 = TOROIDAL_SURFACE ( 'NONE', #4748, 5.100000000000000533, 0.1000000000000001582 ) ;
#11094 = CARTESIAN_POINT ( 'NONE',  ( 0.1983443223721556292, 3.359771601077104375, -4.180704885107414448 ) ) ;
#11095 = CIRCLE ( 'NONE', #12266, 4.000000000000000000 ) ;
#11096 = CARTESIAN_POINT ( 'NONE',  ( 1.500000000000001332, 9.123618653647779187E-16, 7.399999999999999467 ) ) ;
#11097 = CIRCLE ( 'NONE', #6629, 4.000000000000000000 ) ;
#11098 = EDGE_CURVE ( 'NONE', #740, #14327, #3118, .T. ) ;
#11099 = MECHANICAL_DESIGN_GEOMETRIC_PRESENTATION_REPRESENTATION (  '', ( #3565 ), #11113 ) ;
#11100 = DIRECTION ( 'NONE',  ( 0.000000000000000000, 0.000000000000000000, -1.000000000000000000 ) ) ;
#11101 = ADVANCED_FACE ( 'NONE', ( #4112 ), #8463, .F. ) ;
#11102 = ORIENTED_EDGE ( 'NONE', *, *, #12968, .F. ) ;
#11103 = EDGE_LOOP ( 'NONE', ( #10723, #12617, #13595, #1968 ) ) ;
#11104 = CARTESIAN_POINT ( 'NONE',  ( 1.399999999999999689, 0.000000000000000000, 0.000000000000000000 ) ) ;
#11105 = CARTESIAN_POINT ( 'NONE',  ( -5.686050877451574337, -5.768780236673276995, -1.000000000000000000 ) ) ;
#11106 = VECTOR ( 'NONE', #3077, 1000.000000000000000 ) ;
#11107 = LINE ( 'NONE', #10000, #3259 ) ;
#11108 = CARTESIAN_POINT ( 'NONE',  ( 2.500000000000000000, 2.357898499370431722, -2.818925648462311528E-15 ) ) ;
#11109 = CARTESIAN_POINT ( 'NONE',  ( -9.137956343301000928, 374.5525593289319204, 169.9999999999999716 ) ) ;
#11110 = SURFACE_STYLE_FILL_AREA ( #3589 ) ;
#11111 = VERTEX_POINT ( 'NONE', #11024 ) ;
#11112 = AXIS2_PLACEMENT_3D ( 'NONE', #5517, #10012, #12080 ) ;
#11113 =( GEOMETRIC_REPRESENTATION_CONTEXT ( 3 ) GLOBAL_UNCERTAINTY_ASSIGNED_CONTEXT ( ( #10637 ) ) GLOBAL_UNIT_ASSIGNED_CONTEXT ( ( #390, #10600, #482 ) ) REPRESENTATION_CONTEXT ( 'NONE', 'WORKASPACE' ) );
#11114 = CARTESIAN_POINT ( 'NONE',  ( 609.7493509738548028, 188.4639666770506494, 189.3135794259398494 ) ) ;
#11115 = ORIENTED_EDGE ( 'NONE', *, *, #3833, .T. ) ;
#11116 = ORIENTED_EDGE ( 'NONE', *, *, #9438, .T. ) ;
#11117 = LINE ( 'NONE', #996, #11106 ) ;
#11118 = VERTEX_POINT ( 'NONE', #13104 ) ;
#11119 = VECTOR ( 'NONE', #8378, 1000.000000000000000 ) ;
#11120 = DIRECTION ( 'NONE',  ( -3.125627884642896034E-16, 4.141456947151826978E-15, 1.000000000000000000 ) ) ;
#11121 =( REPRESENTATION_RELATIONSHIP ('NONE','NONE', #2822, #5462 ) REPRESENTATION_RELATIONSHIP_WITH_TRANSFORMATION ( #13050 )SHAPE_REPRESENTATION_RELATIONSHIP( ) );
#11122 = FACE_OUTER_BOUND ( 'NONE', #11481, .T. ) ;
#11123 = PRESENTATION_LAYER_ASSIGNMENT (  '', '', ( #8771 ) ) ;
#11124 = ORIENTED_EDGE ( 'NONE', *, *, #1124, .T. ) ;
#11125 = CARTESIAN_POINT ( 'NONE',  ( 610.8620436566991430, 188.5525593289319488, 184.8000000000000682 ) ) ;
#11126 = LINE ( 'NONE', #14591, #6817 ) ;
#11127 = DIRECTION ( 'NONE',  ( -0.2873478855663437748, -0.9578262852211518741, -0.000000000000000000 ) ) ;
#11128 = ORIENTED_EDGE ( 'NONE', *, *, #12621, .T. ) ;
#11129 =( NAMED_UNIT ( * ) SI_UNIT ( $, .STERADIAN. ) SOLID_ANGLE_UNIT ( ) );
#11130 = VERTEX_POINT ( 'NONE', #904 ) ;
#11131 = EDGE_CURVE ( 'NONE', #7099, #11414, #12062, .T. ) ;
#11132 = AXIS2_PLACEMENT_3D ( 'NONE', #6504, #14106, #8411 ) ;
#11133 = VERTEX_POINT ( 'NONE', #4327 ) ;
#11134 = DIRECTION ( 'NONE',  ( 0.000000000000000000, 0.000000000000000000, -1.000000000000000000 ) ) ;
#11135 = DIRECTION ( 'NONE',  ( -0.000000000000000000, -0.000000000000000000, 1.000000000000000000 ) ) ;
#11136 = CARTESIAN_POINT ( 'NONE',  ( 6.500000000000000000, -3.155218591052677990, -0.5622968210053915783 ) ) ;
#11137 = VECTOR ( 'NONE', #5699, 1000.000000000000000 ) ;
#11138 = CARTESIAN_POINT ( 'NONE',  ( 148.9991633467111569, 386.6211705227183870, 190.0000000000000568 ) ) ;
#11139 = CARTESIAN_POINT ( 'NONE',  ( 4.000000000000000000, 2.309401076758515803, -0.4999999999999995559 ) ) ;
#11140 = CARTESIAN_POINT ( 'NONE',  ( 0.1586754815284800446, -2.687817229851461764, 3.344563996438204789 ) ) ;
#11141 = FACE_OUTER_BOUND ( 'NONE', #5285, .T. ) ;
#11142 = EDGE_LOOP ( 'NONE', ( #7990, #14298, #2038, #1043 ) ) ;
#11143 = CARTESIAN_POINT ( 'NONE',  ( 124.4591373975829214, 414.8637913252775320, 8.883675154640809176E-13 ) ) ;
#11144 = DIRECTION ( 'NONE',  ( 0.000000000000000000, 0.000000000000000000, -1.000000000000000000 ) ) ;
#11145 = SHAPE_DEFINITION_REPRESENTATION ( #10176, #5462 ) ;
#11146 = EDGE_CURVE ( 'NONE', #6536, #5286, #690, .T. ) ;
#11148 = CLOSED_SHELL ( 'NONE', ( #3235, #11692, #12396, #14529, #9540, #745, #4795, #13226, #5363, #12224, #9190, #13273, #13324, #10577, #5763, #38, #6638, #14415, #2937, #14283, #5301, #2481, #2884, #206, #2316, #3177, #4349, #12108, #6951, #6807, #9356, #2945, #5530, #2336, #14513, #6659, #4718, #7907, #6574, #12680 ) ) ;
#11147 = CYLINDRICAL_SURFACE ( 'NONE', #14395, 7.000000000000006217 ) ;
#11149 = ORIENTED_EDGE ( 'NONE', *, *, #11623, .T. ) ;
#11150 = ORIENTED_EDGE ( 'NONE', *, *, #9808, .F. ) ;
#11151 = FILL_AREA_STYLE ('',( #5397 ) ) ;
#11152 = CARTESIAN_POINT ( 'NONE',  ( 637.5000000000000000, 160.0000000000000284, -233.5000000000000000 ) ) ;
#11153 = EDGE_CURVE ( 'NONE', #9268, #10050, #8822, .T. ) ;
#11154 = DIRECTION ( 'NONE',  ( -0.9578262852211513190, 0.2873478855663453846, 0.000000000000000000 ) ) ;
#11155 = EDGE_CURVE ( 'NONE', #12082, #8553, #1222, .T. ) ;
#11156 = CARTESIAN_POINT ( 'NONE',  ( -4.424031367838696660, 4.951337798339958240, -6.056431503346038525 ) ) ;
#11157 = ORIENTED_EDGE ( 'NONE', *, *, #8542, .T. ) ;
#11159 = CLOSED_SHELL ( 'NONE', ( #8902, #572, #11438, #13771, #13680, #3919, #12429, #2262, #2959, #13312, #10644, #14166, #6703, #102, #11859, #8082, #3672, #9578, #12821, #13131, #1560 ) ) ;
#11158 = EDGE_CURVE ( 'NONE', #8805, #9145, #6172, .T. ) ;
#11160 = DIRECTION ( 'NONE',  ( 1.000000000000000000, 0.000000000000000000, 0.000000000000000000 ) ) ;
#11161 = EDGE_LOOP ( 'NONE', ( #13875, #826, #2137, #7358 ) ) ;
#11162 = CARTESIAN_POINT ( 'NONE',  ( 133.6739427831727767, 370.3381236739588189, -190.0000000000000000 ) ) ;
#11163 = LINE ( 'NONE', #5550, #13634 ) ;
#11164 = PRESENTATION_STYLE_ASSIGNMENT (( #7772 ) ) ;
#11165 = CARTESIAN_POINT ( 'NONE',  ( 6.534838248920896930, -2.951765777552407766, 5.112608298763836601 ) ) ;
#11166 = ORIENTED_EDGE ( 'NONE', *, *, #11858, .T. ) ;
#11167 = ORIENTED_EDGE ( 'NONE', *, *, #3339, .F. ) ;
#11168 = DIRECTION ( 'NONE',  ( 1.000000000000000000, 0.000000000000000000, -0.000000000000000000 ) ) ;
#11169 = DIRECTION ( 'NONE',  ( 0.000000000000000000, 0.000000000000000000, 1.000000000000000000 ) ) ;
#11170 = ADVANCED_FACE ( 'NONE', ( #14142 ), #19, .F. ) ;
#11171 = B_SPLINE_CURVE_WITH_KNOTS ( 'NONE', 3,
 ( #10066, #8965, #11398, #8075 ),
 .UNSPECIFIED., .F., .F.,
 ( 4, 4 ),
 ( 2.380737582663283482E-07, 0.002336974151641552089 ),
 .UNSPECIFIED. ) ;
#11172 = ADVANCED_FACE ( 'NONE', ( #5138 ), #5935, .T. ) ;
#11173 = FACE_OUTER_BOUND ( 'NONE', #14328, .T. ) ;
#11174 = VERTEX_POINT ( 'NONE', #14356 ) ;
#11175 = ADVANCED_FACE ( 'NONE', ( #4249, #5429, #9930, #9638, #14439, #2167, #11393 ), #4545, .T. ) ;
#11176 = ORIENTED_EDGE ( 'NONE', *, *, #7012, .F. ) ;
#11177 = FACE_BOUND ( 'NONE', #13778, .T. ) ;
#11178 = CARTESIAN_POINT ( 'NONE',  ( 636.9746078850427011, 155.6249658629529620, -210.0000000000000000 ) ) ;
#11179 = CARTESIAN_POINT ( 'NONE',  ( -2.712762565639006418, 3.052587955997511759, -3.430618716626627318 ) ) ;
#11180 = DIRECTION ( 'NONE',  ( -0.2873478855663315623, -0.9578262852211555378, 1.261617073437858516E-13 ) ) ;
#11181 = DIRECTION ( 'NONE',  ( -0.000000000000000000, -0.000000000000000000, -1.000000000000000000 ) ) ;
#11182 = ORIENTED_EDGE ( 'NONE', *, *, #8640, .F. ) ;
#11183 = CARTESIAN_POINT ( 'NONE',  ( 610.0000000000000000, 175.0000000000000568, -210.0000000000000000 ) ) ;
#11184 = ORIENTED_EDGE ( 'NONE', *, *, #13484, .T. ) ;
#11185 = ORIENTED_EDGE ( 'NONE', *, *, #7196, .F. ) ;
#11186 = DIRECTION ( 'NONE',  ( 1.000000000000000000, 0.000000000000000000, 0.000000000000000000 ) ) ;
#11187 = ORIENTED_EDGE ( 'NONE', *, *, #5745, .T. ) ;
#11188 =( BOUNDED_SURFACE ( )  B_SPLINE_SURFACE ( 3, 2, ( 
 ( #6972, #11466, #6905 ),
 ( #17, #11404, #5792 ),
 ( #1443, #8080, #13698 ),
 ( #1359, #5862, #2243 ),
 ( #6750, #1137, #11329 ),
 ( #1219, #7875, #3664 ) ),
 .UNSPECIFIED., .F., .F., .F. ) 
 B_SPLINE_SURFACE_WITH_KNOTS ( ( 4, 2, 4 ),
 ( 3, 3 ),
 ( 0.02368235114939812661, 0.02663560780161266378, 0.02958886445382720443 ),
 ( 0.000000000000000000, 1.000000000000000000 ),
 .UNSPECIFIED. ) 
 GEOMETRIC_REPRESENTATION_ITEM ( )  RATIONAL_B_SPLINE_SURFACE ( (
 ( 1.000000000000000000, 0.8047780980783512117, 1.000000000000000000),
 ( 1.000000000000000000, 0.8123789398383448601, 1.000000000000000000),
 ( 1.000000000000000000, 0.8190677725692530053, 1.000000000000000000),
 ( 1.000000000000000000, 0.8192346316605858547, 1.000000000000000000),
 ( 1.000000000000000000, 0.8126126875065294852, 1.000000000000000000),
 ( 1.000000000000000000, 0.8047712635281869531, 1.000000000000000000) ) ) 
 REPRESENTATION_ITEM ( '' )  SURFACE ( )  );
#11189 = LINE ( 'NONE', #12205, #2343 ) ;
#11190 = CARTESIAN_POINT ( 'NONE',  ( 0.000000000000000000, -2.357898499370432166, 3.035766082959412415E-15 ) ) ;
#11191 = EDGE_LOOP ( 'NONE', ( #5609, #2166 ) ) ;
#11192 = CARTESIAN_POINT ( 'NONE',  ( 6.534838248920897819, 2.951765777552412651, 5.112608298763836601 ) ) ;
#11193 = DIRECTION ( 'NONE',  ( -0.000000000000000000, 0.000000000000000000, -1.000000000000000000 ) ) ;
#11194 = CARTESIAN_POINT ( 'NONE',  ( -4.211140560182196957, -2.431303136016552013, -3.745885042887436178 ) ) ;
#11195 = CARTESIAN_POINT ( 'NONE',  ( 2.000000000000005329, -3.464101615137751722, 0.000000000000000000 ) ) ;
#11196 = SURFACE_STYLE_USAGE ( .BOTH. , #8906 ) ;
#11197 = ORIENTED_EDGE ( 'NONE', *, *, #5984, .F. ) ;
#11198 = CARTESIAN_POINT ( 'NONE',  ( 6.534838248920899595, 5.903531555104835071, -2.091255385257999292E-17 ) ) ;
#11199 = ORIENTED_EDGE ( 'NONE', *, *, #3411, .T. ) ;
#11200 = VERTEX_POINT ( 'NONE', #5781 ) ;
#11201 = DIRECTION ( 'NONE',  ( -0.000000000000000000, 0.000000000000000000, -1.000000000000000000 ) ) ;
#11202 = CARTESIAN_POINT ( 'NONE',  ( 459.7035746174795463, 294.6698471414878782, 187.0000000000000568 ) ) ;
#11203 = CARTESIAN_POINT ( 'NONE',  ( 636.9517704078292581, 167.3095993251051539, -210.0000000000000000 ) ) ;
#11204 = AXIS2_PLACEMENT_3D ( 'NONE', #5102, #9462, #14100 ) ;
#11205 = ADVANCED_FACE ( 'NONE', ( #11177, #1283 ), #13605, .T. ) ;
#11206 = CARTESIAN_POINT ( 'NONE',  ( 640.2500000000000000, 160.0000000000000284, -210.0000000000000000 ) ) ;
#11207 = EDGE_CURVE ( 'NONE', #12163, #9095, #1691, .T. ) ;
#11208 = CARTESIAN_POINT ( 'NONE',  ( 4.000000000000000000, 0.9868501483902631932, -0.09357334158579604100 ) ) ;
#11209 = CARTESIAN_POINT ( 'NONE',  ( -6.837824896291514243, 3.947820044545427454, -6.564402953523716278 ) ) ;
#11210 = DIRECTION ( 'NONE',  ( -0.000000000000000000, -0.000000000000000000, -1.000000000000000000 ) ) ;
#11211 = ORIENTED_EDGE ( 'NONE', *, *, #11276, .F. ) ;
#11212 = CARTESIAN_POINT ( 'NONE',  ( -6.878751942472531411, -3.924677726130930910, -6.573129608219091757 ) ) ;
#11213 = CARTESIAN_POINT ( 'NONE',  ( 726.1975094929949819, 167.5243180396262801, -149.9999999999986358 ) ) ;
#11214 = APPLICATION_PROTOCOL_DEFINITION ( 'draft international standard', 'automotive_design', 1998, #1508 ) ;
#11215 = DIRECTION ( 'NONE',  ( 1.000000000000000000, 0.000000000000000000, 0.000000000000000000 ) ) ;
#11216 = ORIENTED_EDGE ( 'NONE', *, *, #6133, .T. ) ;
#11217 = EDGE_LOOP ( 'NONE', ( #3325, #1357, #3748, #6063 ) ) ;
#11218 = CYLINDRICAL_SURFACE ( 'NONE', #11263, 2.649999999999985700 ) ;
#11219 = CARTESIAN_POINT ( 'NONE',  ( -8.505790995054884007, 418.4210031920614483, 184.7999999999999829 ) ) ;
#11220 = LINE ( 'NONE', #5613, #5637 ) ;
#11221 = EDGE_CURVE ( 'NONE', #12920, #10525, #4702, .T. ) ;
#11222 = CARTESIAN_POINT ( 'NONE',  ( 627.2408731339805854, 284.9098836221799615, -187.0000000000001990 ) ) ;
#11223 = ORIENTED_EDGE ( 'NONE', *, *, #407, .T. ) ;
#11224 = UNCERTAINTY_MEASURE_WITH_UNIT (LENGTH_MEASURE( 1.000000000000000082E-05 ), #851, 'distance_accuracy_value', 'NONE');
#11225 = DIRECTION ( 'NONE',  ( -1.000000000000000000, 0.000000000000000000, 0.000000000000000000 ) ) ;
#11226 = ORIENTED_EDGE ( 'NONE', *, *, #3407, .T. ) ;
#11227 = LINE ( 'NONE', #6878, #3473 ) ;
#11228 = LINE ( 'NONE', #9024, #14115 ) ;
#11229 = SURFACE_STYLE_USAGE ( .BOTH. , #9093 ) ;
#11230 = ADVANCED_FACE ( 'NONE', ( #6742 ), #14192, .T. ) ;
#11231 = CARTESIAN_POINT ( 'NONE',  ( 5.991014884144048480, 4.330127018922193649, 2.500000000000001776 ) ) ;
#11232 = ORIENTED_EDGE ( 'NONE', *, *, #14251, .F. ) ;
#11233 = ORIENTED_EDGE ( 'NONE', *, *, #11085, .F. ) ;
#11234 = CARTESIAN_POINT ( 'NONE',  ( -1.393927851585477606, 4.043713361053528743, -3.526374918436835149 ) ) ;
#11235 = LINE ( 'NONE', #3271, #3752 ) ;
#11236 = CARTESIAN_POINT ( 'NONE',  ( 6.390820841722131718, 5.837016270311240262, 0.1100087447852529932 ) ) ;
#11237 = EDGE_CURVE ( 'NONE', #1071, #12112, #7823, .T. ) ;
#11238 = EDGE_LOOP ( 'NONE', ( #12042, #8844, #8432, #7444 ) ) ;
#11239 = CIRCLE ( 'NONE', #4894, 7.500000000000062172 ) ;
#11240 = EDGE_LOOP ( 'NONE', ( #13092, #8911, #7250, #8095 ) ) ;
#11241 = CARTESIAN_POINT ( 'NONE',  ( 609.6698590453944462, 186.8406770348469195, -188.0140793454688151 ) ) ;
#11242 = LINE ( 'NONE', #5636, #11076 ) ;
#11243 = FACE_OUTER_BOUND ( 'NONE', #1442, .T. ) ;
#11244 = CARTESIAN_POINT ( 'NONE',  ( -2.000000000000006661, 3.464101615137750834, 0.000000000000000000 ) ) ;
#11245 = DIRECTION ( 'NONE',  ( 0.000000000000000000, -0.5000000000000014433, -0.8660254037844378194 ) ) ;
#11246 = EDGE_CURVE ( 'NONE', #7610, #1236, #14500, .T. ) ;
#11247 = ORIENTED_EDGE ( 'NONE', *, *, #8221, .F. ) ;
#11248 = EDGE_CURVE ( 'NONE', #6071, #5821, #1461, .T. ) ;
#11249 = FACE_OUTER_BOUND ( 'NONE', #10582, .T. ) ;
#11250 = ORIENTED_EDGE ( 'NONE', *, *, #14180, .F. ) ;
#11251 = ORIENTED_EDGE ( 'NONE', *, *, #6020, .T. ) ;
#11252 = CARTESIAN_POINT ( 'NONE',  ( 8.500000000000000000, -5.773502691896264416, 0.000000000000000000 ) ) ;
#11253 = VECTOR ( 'NONE', #7223, 1000.000000000000000 ) ;
#11254 = ADVANCED_FACE ( 'NONE', ( #3362 ), #1213, .T. ) ;
#11255 = EDGE_LOOP ( 'NONE', ( #13760, #1822, #6626, #10465 ) ) ;
#11256 = AXIS2_PLACEMENT_3D ( 'NONE', #12134, #3211, #2018 ) ;
#11257 = PRODUCT_DEFINITION ( 'UNKNOWN', '', #8305, #2956 ) ;
#11258 = DIRECTION ( 'NONE',  ( 1.000000000000000000, 0.000000000000000000, 0.000000000000000000 ) ) ;
#11259 = DIRECTION ( 'NONE',  ( -0.9995235871707960351, -0.03086419753086420970, 0.000000000000000000 ) ) ;
#11260 = ORIENTED_EDGE ( 'NONE', *, *, #11602, .T. ) ;
#11261 = FACE_OUTER_BOUND ( 'NONE', #5010, .T. ) ;
#11262 = CARTESIAN_POINT ( 'NONE',  ( 0.000000000000000000, 0.5192545390863916310, 0.000000000000000000 ) ) ;
#11263 = AXIS2_PLACEMENT_3D ( 'NONE', #8798, #12106, #13520 ) ;
#11264 = VECTOR ( 'NONE', #3499, 1000.000000000000000 ) ;
#11265 = CARTESIAN_POINT ( 'NONE',  ( 635.0000000000000000, 160.0000000000000284, -211.0000000000000000 ) ) ;
#11266 = SURFACE_SIDE_STYLE ('',( #3385 ) ) ;
#11267 = ORIENTED_EDGE ( 'NONE', *, *, #13940, .T. ) ;
#11268 = DIRECTION ( 'NONE',  ( -0.000000000000000000, -0.000000000000000000, 1.000000000000000000 ) ) ;
#11269 = ORIENTED_EDGE ( 'NONE', *, *, #683, .F. ) ;
#11270 = ORIENTED_EDGE ( 'NONE', *, *, #4137, .T. ) ;
#11271 = CARTESIAN_POINT ( 'NONE',  ( 6.534838248920899595, 5.903531555104835071, -2.091255385257999292E-17 ) ) ;
#11272 = VECTOR ( 'NONE', #1189, 1000.000000000000000 ) ;
#11274 = AXIS2_PLACEMENT_3D ( 'NONE', #1709, #10774, #9386 ) ;
#11273 = DIRECTION ( 'NONE',  ( -0.000000000000000000, -0.000000000000000000, 1.000000000000000000 ) ) ;
#11275 = CARTESIAN_POINT ( 'NONE',  ( 3.511755186886750923, -2.826662030176382956, -3.597382984111582083 ) ) ;
#11276 = EDGE_CURVE ( 'NONE', #7459, #9269, #2644, .T. ) ;
#11277 = LINE ( 'NONE', #2263, #729 ) ;
#11278 = EDGE_CURVE ( 'NONE', #3772, #13817, #11609, .T. ) ;
#11279 = CARTESIAN_POINT ( 'NONE',  ( 610.0000000000001137, 185.6790804732684421, 184.8000000000000682 ) ) ;
#11280 = DIRECTION ( 'NONE',  ( -0.9578262852211506528, 0.2873478855663477161, -0.000000000000000000 ) ) ;
#11281 = DIRECTION ( 'NONE',  ( -0.9237280213470676626, -0.3830490080632388272, 0.000000000000000000 ) ) ;
#11282 = ORIENTED_EDGE ( 'NONE', *, *, #12700, .F. ) ;
#11283 = CIRCLE ( 'NONE', #2805, 0.5999999999999980904 ) ;
#11284 = VECTOR ( 'NONE', #5686, 1000.000000000000114 ) ;
#11285 = CARTESIAN_POINT ( 'NONE',  ( 0.2813450144774466422, -7.667988119308859041, -6.122077150241856280 ) ) ;
#11286 = DIRECTION ( 'NONE',  ( 0.03086419753086420623, 0.9995235871707959241, 0.000000000000000000 ) ) ;
#11287 = SHAPE_DEFINITION_REPRESENTATION ( #962, #342 ) ;
#11288 = ORIENTED_EDGE ( 'NONE', *, *, #11652, .F. ) ;
#11289 = DIRECTION ( 'NONE',  ( -1.000000000000000000, -0.000000000000000000, -0.000000000000000000 ) ) ;
#11290 = VERTEX_POINT ( 'NONE', #453 ) ;
#11291 = ORIENTED_EDGE ( 'NONE', *, *, #1340, .T. ) ;
#11292 = FILL_AREA_STYLE ('',( #878 ) ) ;
#11293 = CYLINDRICAL_SURFACE ( 'NONE', #12736, 4.799999999999999822 ) ;
#11294 = ADVANCED_FACE ( 'NONE', ( #12575 ), #5937, .F. ) ;
#11295 = DIRECTION ( 'NONE',  ( 0.000000000000000000, 0.000000000000000000, -1.000000000000000000 ) ) ;
#11296 = AXIS2_PLACEMENT_3D ( 'NONE', #10234, #11193, #10081 ) ;
#11297 = PLANE ( 'NONE',  #944 ) ;
#11298 = CARTESIAN_POINT ( 'NONE',  ( 6.357976367241882976, -5.421935536069461214, -0.8264656814054126555 ) ) ;
#11299 = ORIENTED_EDGE ( 'NONE', *, *, #3645, .T. ) ;
#11300 = CARTESIAN_POINT ( 'NONE',  ( 229.2257385731838042, 308.4724102386206255, 177.5999999999999091 ) ) ;
#11301 = EDGE_CURVE ( 'NONE', #5147, #9849, #13717, .T. ) ;
#11302 = CARTESIAN_POINT ( 'NONE',  ( -9.137956343300835726, 416.3137853645748692, 184.7999999999999829 ) ) ;
#11303 = VECTOR ( 'NONE', #2563, 1000.000000000000114 ) ;
#11304 = CARTESIAN_POINT ( 'NONE',  ( 139.8040310085880833, 355.9707293956415697, -187.0000000000000000 ) ) ;
#11305 = AXIS2_PLACEMENT_3D ( 'NONE', #5563, #6813, #13385 ) ;
#11306 = ORIENTED_EDGE ( 'NONE', *, *, #2854, .T. ) ;
#11307 = EDGE_CURVE ( 'NONE', #9876, #14241, #3878, .T. ) ;
#11308 = ORIENTED_EDGE ( 'NONE', *, *, #4681, .F. ) ;
#11309 = FACE_OUTER_BOUND ( 'NONE', #8299, .T. ) ;
#11310 = EDGE_CURVE ( 'NONE', #13548, #14237, #8371, .T. ) ;
#11311 = CARTESIAN_POINT ( 'NONE',  ( 635.0000000000000000, 160.0000000000000284, -217.5000000000000284 ) ) ;
#11312 = AXIS2_PLACEMENT_3D ( 'NONE', #9780, #3268, #6462 ) ;
#11313 = VECTOR ( 'NONE', #540, 1000.000000000000000 ) ;
#11314 = CARTESIAN_POINT ( 'NONE',  ( 6.506891779418575439, 5.826362946429633816, 0.09155664655282295950 ) ) ;
#11315 = CIRCLE ( 'NONE', #14389, 5.000000000000000000 ) ;
#11316 = ORIENTED_EDGE ( 'NONE', *, *, #4319, .F. ) ;
#11317 = CONICAL_SURFACE ( 'NONE', #8022, 2.054999999999999716, 0.7853981633974482790 ) ;
#11318 = VERTEX_POINT ( 'NONE', #6075 ) ;
#11319 = DIRECTION ( 'NONE',  ( 0.000000000000000000, 0.000000000000000000, 1.000000000000000000 ) ) ;
#11320 = DIRECTION ( 'NONE',  ( 0.000000000000000000, 0.000000000000000000, 1.000000000000000000 ) ) ;
#11321 = CARTESIAN_POINT ( 'NONE',  ( -9.511508594537115613, 378.5275384125997107, -190.0000000000000000 ) ) ;
#11322 = CARTESIAN_POINT ( 'NONE',  ( 4.000000000000000000, -2.309401076758514915, -3.433295621305383349 ) ) ;
#11323 = LINE ( 'NONE', #7791, #7381 ) ;
#11324 = EDGE_LOOP ( 'NONE', ( #306, #1349, #12354, #12390 ) ) ;
#11325 = CIRCLE ( 'NONE', #10627, 2.649999999999985700 ) ;
#11326 = CARTESIAN_POINT ( 'NONE',  ( 137.1540310085880776, 355.9707293956415697, 190.0000000000000000 ) ) ;
#11327 = ORIENTED_EDGE ( 'NONE', *, *, #664, .T. ) ;
#11328 = VERTEX_POINT ( 'NONE', #10574 ) ;
#11329 = CARTESIAN_POINT ( 'NONE',  ( 6.357965579934231393, -1.995168835100903593, -5.108766517442098198 ) ) ;
#11330 = EDGE_CURVE ( 'NONE', #6891, #6264, #9014, .T. ) ;
#11331 = CIRCLE ( 'NONE', #8506, 4.199999999999926459 ) ;
#11332 = ORIENTED_EDGE ( 'NONE', *, *, #4263, .F. ) ;
#11333 = ADVANCED_FACE ( 'NONE', ( #4984 ), #2163, .T. ) ;
#11334 = VECTOR ( 'NONE', #5318, 1000.000000000000114 ) ;
#11335 = VECTOR ( 'NONE', #7126, 1000.000000000000000 ) ;
#11336 = LINE ( 'NONE', #11549, #13603 ) ;
#11337 = EDGE_CURVE ( 'NONE', #7099, #4375, #11456, .T. ) ;
#11338 = ORIENTED_EDGE ( 'NONE', *, *, #6579, .F. ) ;
#11339 = CARTESIAN_POINT ( 'NONE',  ( 8.500000000000000000, 0.000000000000000000, 0.000000000000000000 ) ) ;
#11340 = CARTESIAN_POINT ( 'NONE',  ( 0.5590169943749477843, 0.000000000000000000, 0.000000000000000000 ) ) ;
#11341 = AXIS2_PLACEMENT_3D ( 'NONE', #10231, #5729, #10296 ) ;
#11342 = EDGE_CURVE ( 'NONE', #2446, #1880, #2037, .T. ) ;
#11343 = MECHANICAL_DESIGN_GEOMETRIC_PRESENTATION_REPRESENTATION (  '', ( #8283 ), #2869 ) ;
#11344 = FACE_OUTER_BOUND ( 'NONE', #9522, .T. ) ;
#11345 = ORIENTED_EDGE ( 'NONE', *, *, #12601, .F. ) ;
#11346 = CARTESIAN_POINT ( 'NONE',  ( -9.511508594537115613, 378.5275384125997107, -187.0000000000000000 ) ) ;
#11347 = ORIENTED_EDGE ( 'NONE', *, *, #9990, .T. ) ;
#11348 = CIRCLE ( 'NONE', #1918, 20.00000000000001776 ) ;
#11349 = AXIS2_PLACEMENT_3D ( 'NONE', #9921, #13376, #14427 ) ;
#11350 = EDGE_LOOP ( 'NONE', ( #13850, #823, #12595, #11709 ) ) ;
#11351 = LINE ( 'NONE', #9064, #8445 ) ;
#11352 = STYLED_ITEM ( 'NONE', ( #11164 ), #4067 ) ;
#11353 = DIRECTION ( 'NONE',  ( -0.000000000000000000, 1.000000000000000000, 1.224646799147353207E-16 ) ) ;
#11354 = ADVANCED_FACE ( 'NONE', ( #8425 ), #1397, .F. ) ;
#11355 = CARTESIAN_POINT ( 'NONE',  ( 448.9584422793565750, 264.0194060144110608, 190.0000000000000000 ) ) ;
#11356 = ADVANCED_FACE ( 'NONE', ( #5531 ), #1786, .T. ) ;
#11357 = VECTOR ( 'NONE', #2234, 1000.000000000000000 ) ;
#11358 = DIRECTION ( 'NONE',  ( -0.000000000000000000, -0.000000000000000000, -1.000000000000000000 ) ) ;
#11359 = EDGE_CURVE ( 'NONE', #4259, #4325, #1688, .T. ) ;
#11360 = CARTESIAN_POINT ( 'NONE',  ( -6.499999999999999112, -1.280811194704858158, -0.07768058122908438889 ) ) ;
#11361 = DIRECTION ( 'NONE',  ( -0.000000000000000000, 0.000000000000000000, 1.000000000000000000 ) ) ;
#11362 = DIRECTION ( 'NONE',  ( -0.000000000000000000, -0.000000000000000000, 1.000000000000000000 ) ) ;
#11363 = VERTEX_POINT ( 'NONE', #2973 ) ;
#11364 = VERTEX_POINT ( 'NONE', #6195 ) ;
#11365 = DIRECTION ( 'NONE',  ( -0.9237280213470682178, -0.3830490080632377725, 0.000000000000000000 ) ) ;
#11366 = DIRECTION ( 'NONE',  ( -0.000000000000000000, -0.000000000000000000, 1.000000000000000000 ) ) ;
#11367 = CARTESIAN_POINT ( 'NONE',  ( 6.466260427357666707, -5.808561367196026559, 2.605448573279809935E-16 ) ) ;
#11368 = ORIENTED_EDGE ( 'NONE', *, *, #12974, .T. ) ;
#11369 = CARTESIAN_POINT ( 'NONE',  ( -6.500000000000001776, -2.602085213965210642E-15, -5.592027715088707218 ) ) ;
#11370 = ORIENTED_EDGE ( 'NONE', *, *, #966, .F. ) ;
#11371 = EDGE_LOOP ( 'NONE', ( #11647, #1909, #374, #7849 ) ) ;
#11372 = AXIS2_PLACEMENT_3D ( 'NONE', #10692, #3910, #13060 ) ;
#11373 = DIRECTION ( 'NONE',  ( 0.000000000000000000, 0.000000000000000000, -1.000000000000000000 ) ) ;
#11374 = AXIS2_PLACEMENT_3D ( 'NONE', #12716, #10657, #11608 ) ;
#11375 = LINE ( 'NONE', #2583, #4717 ) ;
#11376 = CARTESIAN_POINT ( 'NONE',  ( 716.7018481736364492, 193.3416907550361543, -182.8000000000001535 ) ) ;
#11377 = MECHANICAL_DESIGN_GEOMETRIC_PRESENTATION_REPRESENTATION (  '', ( #9504 ), #2424 ) ;
#11378 = CARTESIAN_POINT ( 'NONE',  ( 6.327632967270661268, -3.313549392876192545, -4.260764098153476453 ) ) ;
#11379 = ORIENTED_EDGE ( 'NONE', *, *, #1582, .T. ) ;
#11380 = CARTESIAN_POINT ( 'NONE',  ( -0.5219667817988843384, 7.204195837485507958, -0.5602453477493336553 ) ) ;
#11381 = DIRECTION ( 'NONE',  ( -1.000000000000000000, 0.000000000000000000, 0.000000000000000000 ) ) ;
#11382 =( NAMED_UNIT ( * ) SI_UNIT ( $, .STERADIAN. ) SOLID_ANGLE_UNIT ( ) );
#11383 = DIRECTION ( 'NONE',  ( 1.000000000000000000, 0.000000000000000000, 0.000000000000000000 ) ) ;
#11384 = EDGE_LOOP ( 'NONE', ( #9792, #13579, #5759, #6039 ) ) ;
#11385 = ORIENTED_EDGE ( 'NONE', *, *, #10063, .T. ) ;
#11386 = CARTESIAN_POINT ( 'NONE',  ( 6.826425371444817536, -2.641426549045776451, -6.344843397090116355 ) ) ;
#11387 = DIRECTION ( 'NONE',  ( 1.000000000000000000, 0.000000000000000000, 0.000000000000000000 ) ) ;
#11388 = DIRECTION ( 'NONE',  ( -1.000000000000000000, -0.000000000000000000, -0.000000000000000000 ) ) ;
#11389 = CONICAL_SURFACE ( 'NONE', #11849, 3.999999999999999112, 0.9599310885968813656 ) ;
#11390 = CARTESIAN_POINT ( 'NONE',  ( 4.211399257449709665, -2.459727064652517114, -3.751161691472417736 ) ) ;
#11391 = ORIENTED_EDGE ( 'NONE', *, *, #3489, .F. ) ;
#11392 = ORIENTED_EDGE ( 'NONE', *, *, #12887, .T. ) ;
#11393 = FACE_BOUND ( 'NONE', #12218, .T. ) ;
#11394 = EDGE_CURVE ( 'NONE', #13817, #11698, #8584, .T. ) ;
#11395 = DIRECTION ( 'NONE',  ( -0.9237280213470676626, -0.3830490080632388272, 0.000000000000000000 ) ) ;
#11396 = DIRECTION ( 'NONE',  ( 0.9578262852211507639, -0.2873478855663477716, -0.000000000000000000 ) ) ;
#11397 = CARTESIAN_POINT ( 'NONE',  ( 707.5067158355135462, 162.6912496279608717, 177.6000000000001648 ) ) ;
#11398 = CARTESIAN_POINT ( 'NONE',  ( -4.407436607684889181E-15, -3.070647092368449016, -2.681483223904198354 ) ) ;
#11399 = SURFACE_SIDE_STYLE ('',( #11110 ) ) ;
#11400 = ORIENTED_EDGE ( 'NONE', *, *, #4200, .F. ) ;
#11401 = DIRECTION ( 'NONE',  ( 0.000000000000000000, 0.000000000000000000, -1.000000000000000000 ) ) ;
#11402 = ORIENTED_EDGE ( 'NONE', *, *, #13992, .F. ) ;
#11403 = ORIENTED_EDGE ( 'NONE', *, *, #13968, .T. ) ;
#11404 = CARTESIAN_POINT ( 'NONE',  ( 6.327625087026977013, 2.033113452596824633, -5.000000000000000000 ) ) ;
#11405 = VERTEX_POINT ( 'NONE', #6226 ) ;
#11406 = DIRECTION ( 'NONE',  ( -9.498873539028489960E-17, 1.000000000000000000, 0.000000000000000000 ) ) ;
#11407 = LINE ( 'NONE', #4704, #3238 ) ;
#11408 = ORIENTED_EDGE ( 'NONE', *, *, #1295, .F. ) ;
#11409 = DIRECTION ( 'NONE',  ( 0.000000000000000000, 0.000000000000000000, 1.000000000000000000 ) ) ;
#11410 = EDGE_CURVE ( 'NONE', #4156, #11405, #2887, .T. ) ;
#11411 = DIRECTION ( 'NONE',  ( 0.000000000000000000, 0.000000000000000000, 1.000000000000000000 ) ) ;
#11412 = CARTESIAN_POINT ( 'NONE',  ( 0.3572655899081595976, 2.309401076758508253, 3.999999999999993339 ) ) ;
#11413 = CARTESIAN_POINT ( 'NONE',  ( 443.6584422793565636, 264.0194060144110608, -187.0000000000000000 ) ) ;
#11414 = VERTEX_POINT ( 'NONE', #7469 ) ;
#11415 = CARTESIAN_POINT ( 'NONE',  ( 0.000000000000000000, 3.464101615137752610, 2.000000000000003997 ) ) ;
#11416 = ORIENTED_EDGE ( 'NONE', *, *, #4005, .T. ) ;
#11417 = EDGE_CURVE ( 'NONE', #10412, #14577, #6960, .T. ) ;
#11418 = ORIENTED_EDGE ( 'NONE', *, *, #9065, .F. ) ;
#11419 = DIRECTION ( 'NONE',  ( -1.000000000000000000, -0.000000000000000000, -0.000000000000000000 ) ) ;
#11420 = CARTESIAN_POINT ( 'NONE',  ( 636.9516943256485320, 152.6905843535471092, -210.0000000000000284 ) ) ;
#11421 = CYLINDRICAL_SURFACE ( 'NONE', #8029, 5.000000000000004441 ) ;
#11422 = CARTESIAN_POINT ( 'NONE',  ( 0.5000000000000000000, -6.429618962271402616, -1.000000000000000000 ) ) ;
#11423 = CARTESIAN_POINT ( 'NONE',  ( 0.000000000000000000, 0.000000000000000000, 0.000000000000000000 ) ) ;
#11424 = CARTESIAN_POINT ( 'NONE',  ( 7.900000000000002132, 0.000000000000000000, 0.000000000000000000 ) ) ;
#11425 = FACE_OUTER_BOUND ( 'NONE', #4309, .T. ) ;
#11426 = ORIENTED_EDGE ( 'NONE', *, *, #3048, .T. ) ;
#11427 = CARTESIAN_POINT ( 'NONE',  ( -9.137956343300736251, 416.3137853645750397, -184.7999999999999829 ) ) ;
#11428 = CARTESIAN_POINT ( 'NONE',  ( -6.500000000000000888, 0.000000000000000000, 0.000000000000000000 ) ) ;
#11429 = DIRECTION ( 'NONE',  ( -0.2873478855663453846, -0.9578262852211513190, 0.000000000000000000 ) ) ;
#11430 = CONTEXT_DEPENDENT_SHAPE_REPRESENTATION ( #9807, #1704 ) ;
#11431 = VERTEX_POINT ( 'NONE', #597 ) ;
#11432 = ADVANCED_FACE ( 'NONE', ( #2201 ), #6566, .T. ) ;
#11433 = CARTESIAN_POINT ( 'NONE',  ( 6.390983631292895595, 3.014665224428354495, 4.999999999999999112 ) ) ;
#11434 = EDGE_LOOP ( 'NONE', ( #7948, #2625, #1999, #10594 ) ) ;
#11435 = EDGE_LOOP ( 'NONE', ( #10865, #7224, #985, #605 ) ) ;
#11436 =( NAMED_UNIT ( * ) PLANE_ANGLE_UNIT ( ) SI_UNIT ( $, .RADIAN. ) );
#11437 = LINE ( 'NONE', #2140, #3312 ) ;
#11438 = ADVANCED_FACE ( 'NONE', ( #5118 ), #7328, .F. ) ;
#11439 = CARTESIAN_POINT ( 'NONE',  ( -3.755786496842903988E-16, -7.505553499465146494, -6.064240316920404439 ) ) ;
#11440 = B_SPLINE_CURVE_WITH_KNOTS ( 'NONE', 3,
 ( #2936, #14157, #9431, #12972, #3005, #3905 ),
 .UNSPECIFIED., .F., .F.,
 ( 4, 2, 4 ),
 ( 0.000000000000000000, 0.001990940508721409253, 0.003981881017442818506 ),
 .UNSPECIFIED. ) ;
#11441 = DIRECTION ( 'NONE',  ( -0.2873478855663454401, -0.9578262852211514300, 0.000000000000000000 ) ) ;
#11442 = DIRECTION ( 'NONE',  ( 1.000000000000000000, 0.000000000000000000, 0.000000000000000000 ) ) ;
#11443 = EDGE_LOOP ( 'NONE', ( #12975, #12413, #2249, #6517, #717 ) ) ;
#11444 = DIRECTION ( 'NONE',  ( -0.2873478855663477161, -0.9578262852211506528, 0.000000000000000000 ) ) ;
#11445 = CARTESIAN_POINT ( 'NONE',  ( 3.250000000000001332, -5.629165124598862313, -5.592027715088713435 ) ) ;
#11446 = DIRECTION ( 'NONE',  ( 0.9945454910858376740, 0.1043037207429823865, 0.000000000000000000 ) ) ;
#11447 = DIRECTION ( 'NONE',  ( -0.000000000000000000, -1.000000000000000000, -0.000000000000000000 ) ) ;
#11448 = VERTEX_POINT ( 'NONE', #5599 ) ;
#11449 = ORIENTED_EDGE ( 'NONE', *, *, #12749, .F. ) ;
#11450 = DIRECTION ( 'NONE',  ( -1.000000000000000000, -0.000000000000000000, -0.000000000000000000 ) ) ;
#11451 = CARTESIAN_POINT ( 'NONE',  ( 708.1388811837595085, 164.7984674554473941, 177.6000000000000512 ) ) ;
#11452 = CARTESIAN_POINT ( 'NONE',  ( 631.0000000000000000, 164.0000000000000284, -225.5000000000000000 ) ) ;
#11453 = ORIENTED_EDGE ( 'NONE', *, *, #6275, .F. ) ;
#11454 = EDGE_CURVE ( 'NONE', #4881, #2797, #8748, .T. ) ;
#11455 = ORIENTED_EDGE ( 'NONE', *, *, #2264, .T. ) ;
#11456 = LINE ( 'NONE', #12640, #263 ) ;
#11457 = CARTESIAN_POINT ( 'NONE',  ( 5.698650001973517121, -4.592339236403569558, -6.344532336093708480 ) ) ;
#11458 = EDGE_CURVE ( 'NONE', #3336, #14510, #9219, .T. ) ;
#11459 = FACE_OUTER_BOUND ( 'NONE', #7055, .T. ) ;
#11460 = FACE_OUTER_BOUND ( 'NONE', #2001, .T. ) ;
#11461 = CARTESIAN_POINT ( 'NONE',  ( 630.5661054975340676, 158.1613647612965110, -211.0000000000000000 ) ) ;
#11462 = PRODUCT_DEFINITION_SHAPE ( 'NONE', 'NONE',  #8374 ) ;
#11463 = ORIENTED_EDGE ( 'NONE', *, *, #8917, .T. ) ;
#11464 = VERTEX_POINT ( 'NONE', #12449 ) ;
#11465 = ORIENTED_EDGE ( 'NONE', *, *, #13879, .F. ) ;
#11466 = CARTESIAN_POINT ( 'NONE',  ( 6.506892073925697240, 2.992473431090949543, -5.000000000000000000 ) ) ;
#11467 = ADVANCED_FACE ( 'NONE', ( #1384 ), #10184, .F. ) ;
#11468 = FACE_OUTER_BOUND ( 'NONE', #5849, .T. ) ;
#11469 = CARTESIAN_POINT ( 'NONE',  ( 2.999999999999999112, 3.464101615137751278, -2.000000000000005773 ) ) ;
#11470 = ORIENTED_EDGE ( 'NONE', *, *, #4543, .F. ) ;
#11471 = LINE ( 'NONE', #5731, #12996 ) ;
#11472 = PLANE ( 'NONE',  #6362 ) ;
#11473 = LINE ( 'NONE', #1368, #8653 ) ;
#11474 = DIRECTION ( 'NONE',  ( -1.000000000000000000, 0.000000000000000000, 0.000000000000000000 ) ) ;
#11475 = PRESENTATION_STYLE_ASSIGNMENT (( #11196 ) ) ;
#11476 = ORIENTED_EDGE ( 'NONE', *, *, #3153, .T. ) ;
#11477 = AXIS2_PLACEMENT_3D ( 'NONE', #9969, #4363, #735 ) ;
#11478 = CARTESIAN_POINT ( 'NONE',  ( 0.3572655899081652042, 4.618802153517012066, 5.829523438926728986E-16 ) ) ;
#11479 = EDGE_LOOP ( 'NONE', ( #6577, #10339, #5294, #12130, #2482, #5428, #3168 ) ) ;
#11480 = AXIS2_PLACEMENT_3D ( 'NONE', #2507, #6797, #11225 ) ;
#11481 = EDGE_LOOP ( 'NONE', ( #6906, #10912, #12876, #12836 ) ) ;
#11482 = CARTESIAN_POINT ( 'NONE',  ( 459.7035746174795463, 294.6698471414878782, -187.0000000000000568 ) ) ;
#11483 = ADVANCED_FACE ( 'NONE', ( #266 ), #9953, .F. ) ;
#11484 = CARTESIAN_POINT ( 'NONE',  ( 641.5485936625826753, 156.2115189222640197, -210.0000000000000284 ) ) ;
#11485 = DIRECTION ( 'NONE',  ( 0.000000000000000000, -0.8660254037844390407, -0.4999999999999993339 ) ) ;
#11486 = VECTOR ( 'NONE', #10937, 1000.000000000000114 ) ;
#11487 = AXIS2_PLACEMENT_3D ( 'NONE', #2531, #10579, #8293 ) ;
#11488 = EDGE_LOOP ( 'NONE', ( #12442, #5263 ) ) ;
#11489 = DIRECTION ( 'NONE',  ( 1.000000000000000000, 0.000000000000000000, -0.000000000000000000 ) ) ;
#11490 = B_SPLINE_CURVE_WITH_KNOTS ( 'NONE', 3,
 ( #8585, #12314, #10659, #11140, #11828, #5532 ),
 .UNSPECIFIED., .F., .F.,
 ( 4, 2, 4 ),
 ( 0.002336974151641552089, 0.003500975885716447588, 0.004664977619791343087 ),
 .UNSPECIFIED. ) ;
#11491 = CARTESIAN_POINT ( 'NONE',  ( -6.500000000000000000, -0.6456425506958733962, 7.521652571618187011E-16 ) ) ;
#11492 = FACE_OUTER_BOUND ( 'NONE', #1450, .T. ) ;
#11493 = LINE ( 'NONE', #336, #5992 ) ;
#11494 = VERTEX_POINT ( 'NONE', #13728 ) ;
#11495 = FACE_OUTER_BOUND ( 'NONE', #2724, .T. ) ;
#11496 = CARTESIAN_POINT ( 'NONE',  ( -4.574783636564919931, -5.228990388887469365, -6.171384342982607407 ) ) ;
#11497 = CARTESIAN_POINT ( 'NONE',  ( 610.0421465541240877, 190.7920056415575516, 186.9999999999999432 ) ) ;
#11498 = EDGE_LOOP ( 'NONE', ( #2926, #573, #11614 ) ) ;
#11499 = CIRCLE ( 'NONE', #10095, 2.041999999999999815 ) ;
#11500 = CARTESIAN_POINT ( 'NONE',  ( 0.5590169943749478954, 0.000000000000000000, 6.750000000000000000 ) ) ;
#11501 = CIRCLE ( 'NONE', #5151, 4.000000000000000000 ) ;
#11502 = ORIENTED_EDGE ( 'NONE', *, *, #10090, .T. ) ;
#11503 = ORIENTED_EDGE ( 'NONE', *, *, #13339, .F. ) ;
#11504 = CARTESIAN_POINT ( 'NONE',  ( 4.000000000000003553, -2.309401076758513138, -3.504271511727127031 ) ) ;
#11505 = CARTESIAN_POINT ( 'NONE',  ( 10.00000000000000000, 386.5596934910894902, 190.0000000000000000 ) ) ;
#11506 = EDGE_CURVE ( 'NONE', #1324, #4609, #12782, .T. ) ;
#11507 = CARTESIAN_POINT ( 'NONE',  ( 637.0568832135862749, 155.4426727739092655, -222.5000000000000000 ) ) ;
#11508 = ADVANCED_FACE ( 'NONE', ( #12676 ), #3599, .T. ) ;
#11509 = EDGE_CURVE ( 'NONE', #3640, #11318, #11571, .T. ) ;
#11510 = DIRECTION ( 'NONE',  ( 0.9578262852211506528, -0.2873478855663477161, -0.000000000000000000 ) ) ;
#11511 = VECTOR ( 'NONE', #13151, 1000.000000000000227 ) ;
#11512 = EDGE_CURVE ( 'NONE', #2328, #2067, #3359, .T. ) ;
#11513 = CARTESIAN_POINT ( 'NONE',  ( -8.505790995055079406, 376.6597771564183859, -190.0000000000000284 ) ) ;
#11514 = ORIENTED_EDGE ( 'NONE', *, *, #9113, .T. ) ;
#11515 = EDGE_CURVE ( 'NONE', #2067, #14449, #13724, .T. ) ;
#11516 = CARTESIAN_POINT ( 'NONE',  ( 227.7315295682384999, 303.4917135554678680, -177.6000000000004775 ) ) ;
#11517 = FACE_OUTER_BOUND ( 'NONE', #11645, .T. ) ;
#11518 = CARTESIAN_POINT ( 'NONE',  ( 635.0000000000000000, 160.0000000000000284, -211.0000000000000000 ) ) ;
#11519 = CARTESIAN_POINT ( 'NONE',  ( 610.0000000000001137, 185.6790804732684421, 187.0000000000000000 ) ) ;
#11520 = ORIENTED_EDGE ( 'NONE', *, *, #7670, .F. ) ;
#11521 = ORIENTED_EDGE ( 'NONE', *, *, #4982, .F. ) ;
#11522 = LINE ( 'NONE', #3797, #632 ) ;
#11523 = CARTESIAN_POINT ( 'NONE',  ( 610.0000000000000000, 145.0000000000000568, 210.0000000000000000 ) ) ;
#11524 = AXIS2_PLACEMENT_3D ( 'NONE', #1159, #39, #10179 ) ;
#11525 = AXIS2_PLACEMENT_3D ( 'NONE', #12237, #2132, #11144 ) ;
#11526 = LINE ( 'NONE', #13676, #2561 ) ;
#11528 = EDGE_CURVE ( 'NONE', #6453, #14577, #3457, .T. ) ;
#11527=STYLED_ITEM('',(#14667),#7462);
#11529 = B_SPLINE_CURVE_WITH_KNOTS ( 'NONE', 3,
 ( #6161, #14057, #9404, #9264, #7035, #7333, #10663, #13995 ),
 .UNSPECIFIED., .F., .F.,
 ( 4, 2, 2, 4 ),
 ( 0.000000000000000000, 0.002450665683189818828, 0.003675998524784728459, 0.004901331366379638524 ),
 .UNSPECIFIED. ) ;
#11530 = ORIENTED_EDGE ( 'NONE', *, *, #10175, .T. ) ;
#11531 = EDGE_CURVE ( 'NONE', #2870, #2398, #12380, .T. ) ;
#11532 = ORIENTED_EDGE ( 'NONE', *, *, #4397, .T. ) ;
#11533 = CARTESIAN_POINT ( 'NONE',  ( 610.2394425817745969, 189.6441153868865399, -186.5350371479513569 ) ) ;
#11534 = DIRECTION ( 'NONE',  ( 0.000000000000000000, -1.000000000000000000, 1.314525273895018220E-15 ) ) ;
#11535 = CARTESIAN_POINT ( 'NONE',  ( 6.436591462021367782, 5.789018756751902473, -4.392644635849238026E-16 ) ) ;
#11536 = CARTESIAN_POINT ( 'NONE',  ( 0.000000000000000000, 0.000000000000000000, 0.000000000000000000 ) ) ;
#11537 = DIRECTION ( 'NONE',  ( 1.000000000000000000, 0.000000000000000000, 0.000000000000000000 ) ) ;
#11538 = ORIENTED_EDGE ( 'NONE', *, *, #3680, .F. ) ;
#11539 = CARTESIAN_POINT ( 'NONE',  ( -4.154094228333542915, 2.398367420968061658, -3.721909803043254694 ) ) ;
#11540 = ORIENTED_EDGE ( 'NONE', *, *, #2963, .T. ) ;
#11541 = ORIENTED_EDGE ( 'NONE', *, *, #5317, .F. ) ;
#11542 = FACE_OUTER_BOUND ( 'NONE', #10173, .T. ) ;
#11543 = AXIS2_PLACEMENT_3D ( 'NONE', #3504, #9185, #2466 ) ;
#11544 = EDGE_CURVE ( 'NONE', #10481, #12598, #3620, .T. ) ;
#11545 = AXIS2_PLACEMENT_3D ( 'NONE', #4354, #9879, #5672 ) ;
#11546 = ADVANCED_FACE ( 'NONE', ( #3687 ), #2490, .T. ) ;
#11547 = VECTOR ( 'NONE', #12494, 1000.000000000000000 ) ;
#11548 = CYLINDRICAL_SURFACE ( 'NONE', #10617, 4.250000000000000000 ) ;
#11549 = CARTESIAN_POINT ( 'NONE',  ( 451.6722694765949768, 316.6998517015743460, 210.0000000000000000 ) ) ;
#11550 = CIRCLE ( 'NONE', #5900, 5.750000000000000000 ) ;
#11551 = ORIENTED_EDGE ( 'NONE', *, *, #12627, .F. ) ;
#11552 = CARTESIAN_POINT ( 'NONE',  ( -8.074769166705394241, 378.0965165842501392, -190.0000000000000000 ) ) ;
#11553 = DIRECTION ( 'NONE',  ( 0.000000000000000000, 0.000000000000000000, 1.000000000000000000 ) ) ;
#11554 = CIRCLE ( 'NONE', #5205, 4.000000000000000000 ) ;
#11555 = DIRECTION ( 'NONE',  ( -0.000000000000000000, -0.000000000000000000, 1.000000000000000000 ) ) ;
#11556 = DIRECTION ( 'NONE',  ( -1.000000000000000000, -0.000000000000000000, -0.000000000000000000 ) ) ;
#11557 = ORIENTED_EDGE ( 'NONE', *, *, #8099, .F. ) ;
#11558 = VECTOR ( 'NONE', #8438, 1000.000000000000000 ) ;
#11559 = LINE ( 'NONE', #7210, #200 ) ;
#11560 = EDGE_LOOP ( 'NONE', ( #9840, #4041 ) ) ;
#11561 = EDGE_LOOP ( 'NONE', ( #6529, #3981, #465, #11850, #11920 ) ) ;
#11563 = FACE_BOUND ( 'NONE', #100, .T. ) ;
#11562 = VECTOR ( 'NONE', #4963, 1000.000000000000000 ) ;
#11564 = VECTOR ( 'NONE', #3695, 1000.000000000000000 ) ;
#11565 = CARTESIAN_POINT ( 'NONE',  ( 0.4465819873852032162, 5.773502691896260863, 3.074436065535979155E-16 ) ) ;
#11567 = AXIS2_PLACEMENT_3D ( 'NONE', #429, #9099, #3422 ) ;
#11566 = DIRECTION ( 'NONE',  ( -0.9114654452181378819, -0.4113766427172327877, 0.000000000000000000 ) ) ;
#11568 = MECHANICAL_DESIGN_GEOMETRIC_PRESENTATION_REPRESENTATION (  '', ( #6842 ), #9455 ) ;
#11569 = ORIENTED_EDGE ( 'NONE', *, *, #6020, .F. ) ;
#11570 = CARTESIAN_POINT ( 'NONE',  ( 0.05140428708382898532, -4.819072548984010496, -1.653121499799247163 ) ) ;
#11571 = LINE ( 'NONE', #7893, #8784 ) ;
#11572 = AXIS2_PLACEMENT_3D ( 'NONE', #10398, #4726, #2428 ) ;
#11573 = CARTESIAN_POINT ( 'NONE',  ( 3.472371940585993855, 2.614027278893175321, -3.320322319201766792 ) ) ;
#11574 = EDGE_CURVE ( 'NONE', #931, #2113, #13290, .T. ) ;
#11575 = EDGE_LOOP ( 'NONE', ( #10456, #9390, #12384, #13429, #3445 ) ) ;
#11576 = AXIS2_PLACEMENT_3D ( 'NONE', #13534, #12482, #5776 ) ;
#11577 = DIRECTION ( 'NONE',  ( 0.9578262852211514300, -0.2873478855663454401, -2.126801590887410810E-15 ) ) ;
#11578 = FILL_AREA_STYLE_COLOUR ( '', #3481 ) ;
#11579 = EDGE_LOOP ( 'NONE', ( #7669, #12068, #9628, #4434 ) ) ;
#11580 = CARTESIAN_POINT ( 'NONE',  ( 6.357987042335823347, 1.995285544161284896, 5.108766985363216051 ) ) ;
#11581 = ORIENTED_EDGE ( 'NONE', *, *, #2425, .T. ) ;
#11582 = VERTEX_POINT ( 'NONE', #5812 ) ;
#11583 = CARTESIAN_POINT ( 'NONE',  ( -8.838721003385150447E-15, -3.857556137907065974, 1.318516776095768339 ) ) ;
#11584 = LINE ( 'NONE', #9456, #10359 ) ;
#11585 = AXIS2_PLACEMENT_3D ( 'NONE', #3277, #13384, #10140 ) ;
#11586 = APPLICATION_CONTEXT ( 'automotive_design' ) ;
#11587 = CARTESIAN_POINT ( 'NONE',  ( 0.1391502195351392857, 2.687187980154705613, 3.345653888883666660 ) ) ;
#11588 = AXIS2_PLACEMENT_3D ( 'NONE', #439, #1412, #1627 ) ;
#11589 = DIRECTION ( 'NONE',  ( -0.2873478855663453846, -0.9578262852211513190, -0.000000000000000000 ) ) ;
#11590 = ADVANCED_FACE ( 'NONE', ( #10400 ), #10472, .T. ) ;
#11591 = VERTEX_POINT ( 'NONE', #3397 ) ;
#11592 = CARTESIAN_POINT ( 'NONE',  ( 2.999999999999999112, 4.000000000000000000, 0.000000000000000000 ) ) ;
#11593 = DIRECTION ( 'NONE',  ( 0.000000000000000000, 0.000000000000000000, -1.000000000000000000 ) ) ;
#11594 = DIRECTION ( 'NONE',  ( 1.000000000000000000, 0.000000000000000000, 0.000000000000000000 ) ) ;
#11595 = VECTOR ( 'NONE', #13019, 1000.000000000000000 ) ;
#11596 = EDGE_CURVE ( 'NONE', #7897, #12715, #404, .T. ) ;
#11597 = CARTESIAN_POINT ( 'NONE',  ( -3.098410542199071749, -7.060458129626440815, -1.000000000000000000 ) ) ;
#11598 = ORIENTED_EDGE ( 'NONE', *, *, #6809, .F. ) ;
#11599 = ORIENTED_EDGE ( 'NONE', *, *, #397, .F. ) ;
#11600 = DIRECTION ( 'NONE',  ( 0.000000000000000000, -1.000000000000000000, -3.344232600703091053E-15 ) ) ;
#11601 = CARTESIAN_POINT ( 'NONE',  ( 635.0000000000000000, 160.0000000000000284, -225.5000000000000000 ) ) ;
#11602 = EDGE_CURVE ( 'NONE', #4517, #173, #8301, .T. ) ;
#11603 = AXIS2_PLACEMENT_3D ( 'NONE', #12781, #7172, #6215 ) ;
#11604 = LINE ( 'NONE', #5997, #9640 ) ;
#11605 = EDGE_CURVE ( 'NONE', #3214, #13261, #7127, .T. ) ;
#11606 = COLOUR_RGB ( '',0.8941176470588234615, 0.8941176470588234615, 0.8941176470588234615 ) ;
#11607 = EDGE_LOOP ( 'NONE', ( #7981, #11216, #10758, #10268 ) ) ;
#11608 = DIRECTION ( 'NONE',  ( 0.000000000000000000, 0.000000000000000000, 1.000000000000000000 ) ) ;
#11609 = LINE ( 'NONE', #6001, #512 ) ;
#11610 = FACE_BOUND ( 'NONE', #1795, .T. ) ;
#11611 = DIRECTION ( 'NONE',  ( 1.000000000000000000, 0.000000000000000000, 0.000000000000000000 ) ) ;
#11612 = DIRECTION ( 'NONE',  ( 0.000000000000000000, 0.000000000000000000, -1.000000000000000000 ) ) ;
#11613 = CARTESIAN_POINT ( 'NONE',  ( -20.63749999999999929, 7.041719095097280880E-16, 5.750000000000000000 ) ) ;
#11614 = ORIENTED_EDGE ( 'NONE', *, *, #9910, .F. ) ;
#11615 = CARTESIAN_POINT ( 'NONE',  ( 639.4338945024659324, 161.8386352387035743, 210.0000000000000000 ) ) ;
#11616 = ORIENTED_EDGE ( 'NONE', *, *, #6726, .F. ) ;
#11617 = VERTEX_POINT ( 'NONE', #2651 ) ;
#11618 = AXIS2_PLACEMENT_3D ( 'NONE', #231, #11181, #2464 ) ;
#11619 = DIRECTION ( 'NONE',  ( 0.000000000000000000, 1.000000000000000000, 0.000000000000000000 ) ) ;
#11620 = EDGE_CURVE ( 'NONE', #7658, #9802, #4071, .T. ) ;
#11621 = ADVANCED_FACE ( 'NONE', ( #2872 ), #567, .F. ) ;
#11622 = CIRCLE ( 'NONE', #13516, 4.000000000000000000 ) ;
#11623 = EDGE_CURVE ( 'NONE', #6413, #13395, #4060, .T. ) ;
#11624 = DIRECTION ( 'NONE',  ( 0.000000000000000000, 0.000000000000000000, 1.000000000000000000 ) ) ;
#11625 = DIRECTION ( 'NONE',  ( 1.000000000000000000, -0.000000000000000000, 0.000000000000000000 ) ) ;
#11626 = DIRECTION ( 'NONE',  ( 1.000000000000000000, 0.000000000000000000, 0.000000000000000000 ) ) ;
#11627 = ORIENTED_EDGE ( 'NONE', *, *, #6446, .F. ) ;
#11628 = CYLINDRICAL_SURFACE ( 'NONE', #12773, 5.200000000000009948 ) ;
#11629 = CARTESIAN_POINT ( 'NONE',  ( 642.0000000000000000, 235.0000000000000284, -233.5000000000000000 ) ) ;
#11630 = DIRECTION ( 'NONE',  ( -1.000000000000000000, 0.000000000000000000, 0.000000000000000000 ) ) ;
#11631 = CARTESIAN_POINT ( 'NONE',  ( -4.197393957002303999, -7.773935952363655451E-14, -3.503767560748929810 ) ) ;
#11632 = ORIENTED_EDGE ( 'NONE', *, *, #9547, .T. ) ;
#11633 = PLANE ( 'NONE',  #4713 ) ;
#11634 = ORIENTED_EDGE ( 'NONE', *, *, #1471, .F. ) ;
#11635 = DIRECTION ( 'NONE',  ( 0.000000000000000000, 0.000000000000000000, -1.000000000000000000 ) ) ;
#11636 = CARTESIAN_POINT ( 'NONE',  ( 610.0000000000000000, 227.4403065089105951, -187.0000000000000000 ) ) ;
#11637 = PLANE ( 'NONE',  #5449 ) ;
#11638 = EDGE_LOOP ( 'NONE', ( #10486, #2824, #1289, #5870 ) ) ;
#11639 = CARTESIAN_POINT ( 'NONE',  ( 0.3106000600989304861, -5.537975084925944813, -0.4079457818577078010 ) ) ;
#11640 = CARTESIAN_POINT ( 'NONE',  ( 635.0000000000000000, 160.0000000000000284, -233.5000000000000000 ) ) ;
#11641 = PLANE ( 'NONE',  #3793 ) ;
#11642 = DIRECTION ( 'NONE',  ( -1.000000000000000000, 0.000000000000000000, 0.000000000000000000 ) ) ;
#11643 = ORIENTED_EDGE ( 'NONE', *, *, #7956, .F. ) ;
#11644 = CARTESIAN_POINT ( 'NONE',  ( 3.500000000000000000, 4.618802153517012954, 0.000000000000000000 ) ) ;
#11645 = EDGE_LOOP ( 'NONE', ( #9321, #6390, #5050, #393, #9959, #2419, #9895, #1342, #1665, #5894, #4107, #9028, #8739, #7700, #12244, #9949 ) ) ;
#11646 = CARTESIAN_POINT ( 'NONE',  ( 4.197393957002303999, 0.8151795401431359833, -3.503767560748935139 ) ) ;
#11647 = ORIENTED_EDGE ( 'NONE', *, *, #9994, .T. ) ;
#11648 = ORIENTED_EDGE ( 'NONE', *, *, #1510, .T. ) ;
#11649 = SURFACE_STYLE_FILL_AREA ( #3698 ) ;
#11650 = CARTESIAN_POINT ( 'NONE',  ( -8.505790995054884007, 418.4210031920614483, 184.7999999999999829 ) ) ;
#11651 = CARTESIAN_POINT ( 'NONE',  ( -6.539196172010138142, -3.775406670193829584, -6.286444963328671420 ) ) ;
#11652 = EDGE_CURVE ( 'NONE', #6727, #12397, #1234, .T. ) ;
#11653 = CARTESIAN_POINT ( 'NONE',  ( -4.211140560182196957, 2.431303136016537803, -3.745885042887433514 ) ) ;
#11654 = EDGE_CURVE ( 'NONE', #14327, #2290, #6069, .T. ) ;
#11655 = DIRECTION ( 'NONE',  ( -1.000000000000000000, 0.000000000000000000, 0.000000000000000000 ) ) ;
#11656 = UNCERTAINTY_MEASURE_WITH_UNIT (LENGTH_MEASURE( 1.000000000000000082E-05 ), #13305, 'distance_accuracy_value', 'NONE');
#11657 = CARTESIAN_POINT ( 'NONE',  ( 641.0000000000000000, 154.0000000000000568, 187.5000000000000000 ) ) ;
#11658 = ORIENTED_EDGE ( 'NONE', *, *, #3254, .T. ) ;
#11659 = CARTESIAN_POINT ( 'NONE',  ( -10.00000000000000000, 10.00000000000000178, -210.0020000000000095 ) ) ;
#11660 = FACE_BOUND ( 'NONE', #14550, .T. ) ;
#11661 = DIRECTION ( 'NONE',  ( 0.000000000000000000, 0.000000000000000000, 1.000000000000000000 ) ) ;
#11662 = CYLINDRICAL_SURFACE ( 'NONE', #2840, 3.399999999999999911 ) ;
#11663 = ORIENTED_EDGE ( 'NONE', *, *, #14063, .F. ) ;
#11664 = ORIENTED_EDGE ( 'NONE', *, *, #2218, .T. ) ;
#11665 = LINE ( 'NONE', #2679, #144 ) ;
#11666 = DIRECTION ( 'NONE',  ( 0.000000000000000000, 1.000000000000000000, 0.000000000000000000 ) ) ;
#11667 = DIRECTION ( 'NONE',  ( -0.000000000000000000, -0.000000000000000000, 1.000000000000000000 ) ) ;
#11668 = EDGE_CURVE ( 'NONE', #4861, #542, #5088, .T. ) ;
#11669 = B_SPLINE_CURVE_WITH_KNOTS ( 'NONE', 3,
 ( #1947, #5200, #9627, #9777, #6297 ),
 .UNSPECIFIED., .F., .F.,
 ( 4, 1, 4 ),
 ( 0.000000000000000000, 0.002309401076758505356, 0.004618802153517010713 ),
 .UNSPECIFIED. ) ;
#11670 = FACE_OUTER_BOUND ( 'NONE', #6016, .T. ) ;
#11671 = EDGE_LOOP ( 'NONE', ( #6982, #9409, #13611 ) ) ;
#11672 = DIRECTION ( 'NONE',  ( -1.000000000000000000, 0.000000000000000000, 0.000000000000000000 ) ) ;
#11673 = CARTESIAN_POINT ( 'NONE',  ( 6.403457969954072126, -2.888443235695472122, -5.002930439003193896 ) ) ;
#11674 = DIRECTION ( 'NONE',  ( 0.9578262852211514300, -0.2873478855663454401, -0.000000000000000000 ) ) ;
#11675 = EDGE_CURVE ( 'NONE', #9054, #11431, #8551, .T. ) ;
#11676 = CARTESIAN_POINT ( 'NONE',  ( 640.2500000000000000, 160.0000000000000284, -210.0000000000000000 ) ) ;
#11677 = LINE ( 'NONE', #9263, #3011 ) ;
#11678 = FACE_OUTER_BOUND ( 'NONE', #5641, .T. ) ;
#11679 = ORIENTED_EDGE ( 'NONE', *, *, #1036, .T. ) ;
#11680 = CARTESIAN_POINT ( 'NONE',  ( -10.00000000000000000, 371.6790804732683569, -187.0000000000000000 ) ) ;
#11681 = ORIENTED_EDGE ( 'NONE', *, *, #970, .T. ) ;
#11682 = ORIENTED_EDGE ( 'NONE', *, *, #8993, .T. ) ;
#11683 = CARTESIAN_POINT ( 'NONE',  ( -4.000000000000000000, 0.1981133338132459731, 2.096406544454392723E-17 ) ) ;
#11684 = EDGE_CURVE ( 'NONE', #6458, #8478, #9726, .T. ) ;
#11685 = DIRECTION ( 'NONE',  ( 0.000000000000000000, 0.000000000000000000, 1.000000000000000000 ) ) ;
#11686 = CARTESIAN_POINT ( 'NONE',  ( 0.1481481481481481122, -4.797713218419819903, -1.000000000000000000 ) ) ;
#11687 = DIRECTION ( 'NONE',  ( 0.000000000000000000, 0.000000000000000000, -1.000000000000000000 ) ) ;
#11688 = ORIENTED_EDGE ( 'NONE', *, *, #12220, .F. ) ;
#11689 = ADVANCED_FACE ( 'NONE', ( #7218 ), #3761, .F. ) ;
#11690 = DIRECTION ( 'NONE',  ( 1.000000000000000000, 2.312964634635740689E-15, 0.000000000000000000 ) ) ;
#11691 = LINE ( 'NONE', #9420, #13440 ) ;
#11692 = ADVANCED_FACE ( 'NONE', ( #11706 ), #1604, .F. ) ;
#11693 = CARTESIAN_POINT ( 'NONE',  ( 0.000000000000000000, 0.000000000000000000, -4.694516984716113228 ) ) ;
#11694 = SHAPE_REPRESENTATION_RELATIONSHIP ( 'NONE' , 'NONE' ,  #6959, #11811 ) ;
#11695 = ORIENTED_EDGE ( 'NONE', *, *, #4385, .F. ) ;
#11696 = ADVANCED_FACE ( 'NONE', ( #7289 ), #5711, .T. ) ;
#11697 = FACE_BOUND ( 'NONE', #10006, .T. ) ;
#11698 = VERTEX_POINT ( 'NONE', #14020 ) ;
#11699 = CARTESIAN_POINT ( 'NONE',  ( 705.2654023280961155, 165.6605111121450591, -177.6000000000005627 ) ) ;
#11700 = FACE_OUTER_BOUND ( 'NONE', #12272, .T. ) ;
#11701 = DIRECTION ( 'NONE',  ( 0.000000000000000000, 0.4999999999999990563, -0.8660254037844391517 ) ) ;
#11702 = ORIENTED_EDGE ( 'NONE', *, *, #11840, .F. ) ;
#11703 = CARTESIAN_POINT ( 'NONE',  ( 610.0000000000001137, 191.1080398579019288, 190.0300000000000296 ) ) ;
#11704 = AXIS2_PLACEMENT_3D ( 'NONE', #11300, #10122, #11444 ) ;
#11705 = CIRCLE ( 'NONE', #9362, 6.975000000000000533 ) ;
#11706 = FACE_OUTER_BOUND ( 'NONE', #4535, .T. ) ;
#11707 = CARTESIAN_POINT ( 'NONE',  ( 6.500000000000000000, 1.602771114417268050, -0.1495523863686167576 ) ) ;
#11708 = CARTESIAN_POINT ( 'NONE',  ( 4.140404888673277384, 2.228338276487440428, -3.686887068327033390 ) ) ;
#11709 = ORIENTED_EDGE ( 'NONE', *, *, #3455, .F. ) ;
#11710 = FILL_AREA_STYLE_COLOUR ( '', #440 ) ;
#11711 = DIRECTION ( 'NONE',  ( -7.930164461608254918E-15, 1.000000000000000000, 0.000000000000000000 ) ) ;
#11712 = ORIENTED_EDGE ( 'NONE', *, *, #3460, .T. ) ;
#11713 = DIRECTION ( 'NONE',  ( 0.000000000000000000, 0.000000000000000000, 1.000000000000000000 ) ) ;
#11714 = ORIENTED_EDGE ( 'NONE', *, *, #10808, .T. ) ;
#11715 = ORIENTED_EDGE ( 'NONE', *, *, #13577, .T. ) ;
#11716 = CARTESIAN_POINT ( 'NONE',  ( 3.500000000000000000, 2.309401076758508253, 3.999999999999993339 ) ) ;
#11717 = VECTOR ( 'NONE', #11758, 1000.000000000000000 ) ;
#11718 = ADVANCED_FACE ( 'NONE', ( #14521 ), #13337, .T. ) ;
#11719 = DIRECTION ( 'NONE',  ( 0.000000000000000000, -1.000000000000000000, 0.000000000000000000 ) ) ;
#11720 = CARTESIAN_POINT ( 'NONE',  ( 4.211405965630455661, 2.460463115436283932, -3.751298928144577882 ) ) ;
#11721 = EDGE_CURVE ( 'NONE', #10481, #4991, #8775, .T. ) ;
#11722 = CARTESIAN_POINT ( 'NONE',  ( 164.3243839102495656, 402.9042173714779551, 210.0000000000000000 ) ) ;
#11723 = VERTEX_POINT ( 'NONE', #9801 ) ;
#11724 = AXIS2_PLACEMENT_3D ( 'NONE', #3939, #8427, #7186 ) ;
#11725 = DIRECTION ( 'NONE',  ( -1.000000000000000000, -2.523234146875633539E-14, 0.000000000000000000 ) ) ;
#11726 = CARTESIAN_POINT ( 'NONE',  ( 631.0000000000000000, 164.0000000000000284, -225.5000000000000000 ) ) ;
#11727 = CARTESIAN_POINT ( 'NONE',  ( 0.000000000000000000, 0.000000000000000000, 0.000000000000000000 ) ) ;
#11728 = CARTESIAN_POINT ( 'NONE',  ( 6.403457969954070350, 2.888443235695463240, 5.002930439003193008 ) ) ;
#11729 = ORIENTED_EDGE ( 'NONE', *, *, #7925, .F. ) ;
#11730 = EDGE_LOOP ( 'NONE', ( #8548, #10543, #4608, #13664 ) ) ;
#11731 = DIRECTION ( 'NONE',  ( 0.000000000000000000, -0.000000000000000000, 1.000000000000000000 ) ) ;
#11732 = CARTESIAN_POINT ( 'NONE',  ( 635.0000000000000000, 160.0000000000000284, 211.0000000000000000 ) ) ;
#11733 = CARTESIAN_POINT ( 'NONE',  ( 2.000000000000008882, 3.464101615137749945, 0.000000000000000000 ) ) ;
#11734 = VECTOR ( 'NONE', #10847, 1000.000000000000227 ) ;
#11735 = AXIS2_PLACEMENT_3D ( 'NONE', #5339, #890, #6590 ) ;
#11736 = AXIS2_PLACEMENT_3D ( 'NONE', #8493, #9537, #3862 ) ;
#11737 = CARTESIAN_POINT ( 'NONE',  ( 639.0000000000000000, 156.0000000000000000, -225.5000000000000000 ) ) ;
#11738 = ORIENTED_EDGE ( 'NONE', *, *, #242, .T. ) ;
#11739 = FACE_OUTER_BOUND ( 'NONE', #912, .T. ) ;
#11740 = CARTESIAN_POINT ( 'NONE',  ( 6.436591462021367782, -2.894509378375955677, -5.013437306331753440 ) ) ;
#11741 = CARTESIAN_POINT ( 'NONE',  ( 706.6446721788148579, 159.8177707722968819, -177.6000000000004775 ) ) ;
#11742 = CONICAL_SURFACE ( 'NONE', #4456, 2.055000000000000160, 0.7853981633974639331 ) ;
#11743 = LINE ( 'NONE', #1567, #6786 ) ;
#11744 = CARTESIAN_POINT ( 'NONE',  ( 112.9652219749295341, 376.5507399164317803, 210.0000000000000000 ) ) ;
#11745 = LINE ( 'NONE', #11613, #12091 ) ;
#11746 = EDGE_CURVE ( 'NONE', #3675, #2766, #7605, .T. ) ;
#11747 = EDGE_CURVE ( 'NONE', #6264, #6891, #6890, .T. ) ;
#11748 = ORIENTED_EDGE ( 'NONE', *, *, #7670, .T. ) ;
#11749 = AXIS2_PLACEMENT_3D ( 'NONE', #1199, #5709, #6599 ) ;
#11750 = DIRECTION ( 'NONE',  ( -1.000000000000000000, -0.000000000000000000, -0.000000000000000000 ) ) ;
#11751 = TOROIDAL_SURFACE ( 'NONE', #7984, 8.331345277524542681, 0.6186547224754559426 ) ;
#11752 = EDGE_LOOP ( 'NONE', ( #196, #2031, #8815, #702 ) ) ;
#11753 = ORIENTED_EDGE ( 'NONE', *, *, #4776, .F. ) ;
#11754 = DIRECTION ( 'NONE',  ( 0.000000000000000000, 1.000000000000000000, 0.000000000000000000 ) ) ;
#11755 = CARTESIAN_POINT ( 'NONE',  ( 0.2499999999999966416, -8.096141056083448362, 0.000000000000000000 ) ) ;
#11756 = CARTESIAN_POINT ( 'NONE',  ( -31.74999999999995737, 0.000000000000000000, 4.250000000000000000 ) ) ;
#11757 = AXIS2_PLACEMENT_3D ( 'NONE', #8628, #9812, #511 ) ;
#11758 = DIRECTION ( 'NONE',  ( 0.000000000000000000, 1.000000000000000000, 0.000000000000000000 ) ) ;
#11759 = AXIS2_PLACEMENT_3D ( 'NONE', #6415, #14456, #630 ) ;
#11760 = ORIENTED_EDGE ( 'NONE', *, *, #8876, .T. ) ;
#11761 = CARTESIAN_POINT ( 'NONE',  ( 112.3905262037967105, 374.6350873459881541, -182.8000000000008640 ) ) ;
#11762 = CARTESIAN_POINT ( 'NONE',  ( 6.826581433398040133, -2.695947255479557381, -6.331032031596317999 ) ) ;
#11763 = DIRECTION ( 'NONE',  ( -1.000000000000000000, 0.000000000000000000, 0.000000000000000000 ) ) ;
#11764 = EDGE_CURVE ( 'NONE', #13545, #11084, #4346, .T. ) ;
#11765 = ORIENTED_EDGE ( 'NONE', *, *, #3686, .F. ) ;
#11766 = CIRCLE ( 'NONE', #8005, 5.384454397937118664 ) ;
#11767 = LINE ( 'NONE', #1744, #10353 ) ;
#11768 = CARTESIAN_POINT ( 'NONE',  ( 6.466260427357672924, 2.904280683598008839, -5.030361703432631337 ) ) ;
#11769 = CONTEXT_DEPENDENT_SHAPE_REPRESENTATION ( #2050, #9594 ) ;
#11770 = ORIENTED_EDGE ( 'NONE', *, *, #8165, .T. ) ;
#11771 = EDGE_CURVE ( 'NONE', #2441, #13081, #6488, .T. ) ;
#11772 = AXIS2_PLACEMENT_3D ( 'NONE', #330, #402, #9066 ) ;
#11773 = AXIS2_PLACEMENT_3D ( 'NONE', #10959, #834, #5352 ) ;
#11774 = LINE ( 'NONE', #12825, #6338 ) ;
#11775 = ADVANCED_FACE ( 'NONE', ( #7812 ), #3227, .T. ) ;
#11776 = ADVANCED_BREP_SHAPE_REPRESENTATION ( '', ( #2170, #9440 ), #10888 ) ;
#11777 = DIRECTION ( 'NONE',  ( 0.000000000000000000, 0.000000000000000000, 1.000000000000000000 ) ) ;
#11778 = AXIS2_PLACEMENT_3D ( 'NONE', #6747, #7932, #8970 ) ;
#11779 = DIRECTION ( 'NONE',  ( -0.000000000000000000, -0.000000000000000000, 1.000000000000000000 ) ) ;
#11780 = ADVANCED_FACE ( 'NONE', ( #10836, #12005 ), #13274, .T. ) ;
#11781 = VERTEX_POINT ( 'NONE', #4193 ) ;
#11782 = DIRECTION ( 'NONE',  ( -0.9578262852211513190, 0.2873478855663453846, 0.000000000000000000 ) ) ;
#11783 = AXIS2_PLACEMENT_3D ( 'NONE', #9051, #8144, #2630 ) ;
#11784 = CIRCLE ( 'NONE', #4029, 8.099999999999999645 ) ;
#11785 = CARTESIAN_POINT ( 'NONE',  ( 610.2366331756301179, 189.6374102278066971, -186.5502271136477361 ) ) ;
#11786 = CARTESIAN_POINT ( 'NONE',  ( 6.500000000000000888, 0.3213925021621134026, 6.640738306473707756E-16 ) ) ;
#11787 = FACE_OUTER_BOUND ( 'NONE', #9725, .T. ) ;
#11788 = VERTEX_POINT ( 'NONE', #4410 ) ;
#11789 = FILL_AREA_STYLE ('',( #11710 ) ) ;
#11790 = DIRECTION ( 'NONE',  ( 0.000000000000000000, 0.5000000000000008882, -0.8660254037844380415 ) ) ;
#11791 = ORIENTED_EDGE ( 'NONE', *, *, #5732, .F. ) ;
#11792 = CIRCLE ( 'NONE', #1196, 5.000000000000004441 ) ;
#11793 = ORIENTED_EDGE ( 'NONE', *, *, #31, .T. ) ;
#11794 = VECTOR ( 'NONE', #10562, 1000.000000000000114 ) ;
#11795 = EDGE_LOOP ( 'NONE', ( #9736, #1732, #3929, #14091 ) ) ;
#11796 = DIRECTION ( 'NONE',  ( -0.2873478855663497700, -0.9578262852211499867, 0.000000000000000000 ) ) ;
#11797 = EDGE_CURVE ( 'NONE', #2291, #11290, #6666, .T. ) ;
#11798 = AXIS2_PLACEMENT_3D ( 'NONE', #10468, #4643, #13944 ) ;
#11799 = EDGE_CURVE ( 'NONE', #5692, #2242, #1720, .T. ) ;
#11800 = COLOUR_RGB ( '',0.8941176470588234615, 0.8941176470588234615, 0.8941176470588234615 ) ;
#11801 = CARTESIAN_POINT ( 'NONE',  ( 6.499999999999999112, -3.752776749732576356, -0.8000000000000003775 ) ) ;
#11802 = FACE_OUTER_BOUND ( 'NONE', #6546, .T. ) ;
#11803 = EDGE_CURVE ( 'NONE', #10470, #9145, #4128, .T. ) ;
#11804 = VECTOR ( 'NONE', #4805, 1000.000000000000000 ) ;
#11805 = DIRECTION ( 'NONE',  ( -0.000000000000000000, 0.000000000000000000, -1.000000000000000000 ) ) ;
#11806 = VECTOR ( 'NONE', #4879, 1000.000000000000114 ) ;
#11807 = FACE_OUTER_BOUND ( 'NONE', #762, .T. ) ;
#11808 = VERTEX_POINT ( 'NONE', #5241 ) ;
#11809 = VECTOR ( 'NONE', #6190, 1000.000000000000000 ) ;
#11810 = STYLED_ITEM ( 'NONE', ( #1058 ), #11776 ) ;
#11811 = ADVANCED_BREP_SHAPE_REPRESENTATION ( '', ( #7155, #9440 ), #6853 ) ;
#11812 = CARTESIAN_POINT ( 'NONE',  ( 0.4465819873852032162, 5.773502691896260863, 3.074436065535979155E-16 ) ) ;
#11813 = FACE_OUTER_BOUND ( 'NONE', #193, .T. ) ;
#11814 = APPLICATION_PROTOCOL_DEFINITION ( 'draft international standard', 'automotive_design', 1998, #9333 ) ;
#11815 = LINE ( 'NONE', #1844, #7794 ) ;
#11816 = VERTEX_POINT ( 'NONE', #792 ) ;
#11817 = ORIENTED_EDGE ( 'NONE', *, *, #12950, .T. ) ;
#11818 = AXIS2_PLACEMENT_3D ( 'NONE', #12193, #6242, #14285 ) ;
#11819 = DIRECTION ( 'NONE',  ( -0.000000000000000000, -0.000000000000000000, 1.000000000000000000 ) ) ;
#11820 = CARTESIAN_POINT ( 'NONE',  ( 708.1388811837593948, 164.7984674554467404, 177.6000000000001648 ) ) ;
#11821 = DIRECTION ( 'NONE',  ( 0.8660254037844382635, -0.5000000000000006661, 0.000000000000000000 ) ) ;
#11822 =( GEOMETRIC_REPRESENTATION_CONTEXT ( 3 ) GLOBAL_UNCERTAINTY_ASSIGNED_CONTEXT ( ( #14315 ) ) GLOBAL_UNIT_ASSIGNED_CONTEXT ( ( #2373, #9025, #11382 ) ) REPRESENTATION_CONTEXT ( 'NONE', 'WORKASPACE' ) );
#11823 = CARTESIAN_POINT ( 'NONE',  ( 632.5000000000001137, 160.0000000000000284, -217.5000000000000284 ) ) ;
#11824 = ORIENTED_EDGE ( 'NONE', *, *, #77, .T. ) ;
#11825 = AXIS2_PLACEMENT_3D ( 'NONE', #11423, #43, #9001 ) ;
#11826 = LINE ( 'NONE', #10725, #12561 ) ;
#11827 = CARTESIAN_POINT ( 'NONE',  ( -4.490121653395046097E-15, -3.660093687634849768, -1.660531772554302288 ) ) ;
#11828 = CARTESIAN_POINT ( 'NONE',  ( 0.2484800633749931209, -2.497823135841249709, 3.673643420401906390 ) ) ;
#11829 = CARTESIAN_POINT ( 'NONE',  ( 0.2486750293982372684, -1.933232340707399910, -4.000000000000000000 ) ) ;
#11830 = CYLINDRICAL_SURFACE ( 'NONE', #9872, 2.396904916527699214 ) ;
#11831 = SURFACE_SIDE_STYLE ('',( #1436 ) ) ;
#11832 = PRODUCT_DEFINITION_SHAPE ( 'NONE', 'NONE',  #14628 ) ;
#11833 = VERTEX_POINT ( 'NONE', #12085 ) ;
#11834 = AXIS2_PLACEMENT_3D ( 'NONE', #10933, #6273, #2897 ) ;
#11835 = ORIENTED_EDGE ( 'NONE', *, *, #12372, .F. ) ;
#11836 = VERTEX_POINT ( 'NONE', #7732 ) ;
#11837 = CARTESIAN_POINT ( 'NONE',  ( -4.000000000000000000, 2.309401076758498483, -0.4999999999999927280 ) ) ;
#11838 = AXIS2_PLACEMENT_3D ( 'NONE', #10165, #5736, #12522 ) ;
#11839 = DIRECTION ( 'NONE',  ( -0.000000000000000000, -0.000000000000000000, 1.000000000000000000 ) ) ;
#11840 = EDGE_CURVE ( 'NONE', #9048, #2225, #12793, .T. ) ;
#11841 = DIRECTION ( 'NONE',  ( 0.2873478855663418874, 0.9578262852211524292, 0.000000000000000000 ) ) ;
#11842 = CARTESIAN_POINT ( 'NONE',  ( 0.000000000000000000, 0.000000000000000000, -5.000000000000000000 ) ) ;
#11843 = EDGE_LOOP ( 'NONE', ( #14597, #135, #13692, #14190, #4553 ) ) ;
#11844 = DIRECTION ( 'NONE',  ( 0.2873478855663396114, 0.9578262852211530953, 0.000000000000000000 ) ) ;
#11845 = CARTESIAN_POINT ( 'NONE',  ( 7.240873133980776366, 470.9098836221796773, 190.0000000000001990 ) ) ;
#11846 = CARTESIAN_POINT ( 'NONE',  ( -2.836893136758495970, -3.208949435745868328, -3.505054077164885484 ) ) ;
#11847 = CARTESIAN_POINT ( 'NONE',  ( 5.000000000000000888, 4.250000000000000000, 0.000000000000000000 ) ) ;
#11848 =( NAMED_UNIT ( * ) PLANE_ANGLE_UNIT ( ) SI_UNIT ( $, .RADIAN. ) );
#11849 = AXIS2_PLACEMENT_3D ( 'NONE', #537, #4989, #7118 ) ;
#11850 = ORIENTED_EDGE ( 'NONE', *, *, #14209, .F. ) ;
#11851 = VECTOR ( 'NONE', #13363, 1000.000000000000000 ) ;
#11852 = DIRECTION ( 'NONE',  ( 0.000000000000000000, 0.000000000000000000, 1.000000000000000000 ) ) ;
#11853 = CARTESIAN_POINT ( 'NONE',  ( 610.3331342679523459, 189.2775297294220991, 186.2537089296249349 ) ) ;
#11854 = ITEM_DEFINED_TRANSFORMATION ( 'NONE', 'NONE', #35,  #9440 ) ;
#11855 = ORIENTED_EDGE ( 'NONE', *, *, #583, .T. ) ;
#11856 = DIRECTION ( 'NONE',  ( 1.000000000000000000, 0.000000000000000000, 0.000000000000000000 ) ) ;
#11857 = CARTESIAN_POINT ( 'NONE',  ( -1.654100357141833219E-15, 3.857556137907077964, -1.318516776095772336 ) ) ;
#11858 = EDGE_CURVE ( 'NONE', #4822, #11011, #6204, .T. ) ;
#11859 = ADVANCED_FACE ( 'NONE', ( #12213 ), #8905, .F. ) ;
#11860 = DIRECTION ( 'NONE',  ( -1.000000000000000000, 0.000000000000000000, -0.000000000000000000 ) ) ;
#11861 = VERTEX_POINT ( 'NONE', #8617 ) ;
#11862 = DIRECTION ( 'NONE',  ( 1.000000000000000000, 0.000000000000000000, -0.000000000000000000 ) ) ;
#11863 = CARTESIAN_POINT ( 'NONE',  ( 610.1812141201095301, 189.9029010627875493, -186.7093446292720387 ) ) ;
#11864 = CARTESIAN_POINT ( 'NONE',  ( 0.1983443223721549353, -3.359771601077103487, 4.180704885107415336 ) ) ;
#11865 = LINE ( 'NONE', #12351, #6328 ) ;
#11866 = ORIENTED_EDGE ( 'NONE', *, *, #5347, .F. ) ;
#11867 = ADVANCED_FACE ( 'NONE', ( #13121 ), #3089, .F. ) ;
#11868 = CARTESIAN_POINT ( 'NONE',  ( 6.244297270354684848, -1.799661607120071246E-11, -5.105276777067894400 ) ) ;
#11869 = CARTESIAN_POINT ( 'NONE',  ( 6.244004651191001010, 4.178905357954649347, -2.972460101650455488 ) ) ;
#11870 = EDGE_LOOP ( 'NONE', ( #1698, #11793, #1291, #7793 ) ) ;
#11871 =( REPRESENTATION_RELATIONSHIP ('NONE','NONE', #2822, #9337 ) REPRESENTATION_RELATIONSHIP_WITH_TRANSFORMATION ( #9300 )SHAPE_REPRESENTATION_RELATIONSHIP( ) );
#11872 = ORIENTED_EDGE ( 'NONE', *, *, #5484, .T. ) ;
#11873 = CARTESIAN_POINT ( 'NONE',  ( 102.3333502089745650, 341.1111673632485122, 1.352973838917536986E-12 ) ) ;
#11874 = CARTESIAN_POINT ( 'NONE',  ( 0.2499999999999966416, -8.096141056083448362, -1.000000000000000000 ) ) ;
#11875 = EDGE_CURVE ( 'NONE', #6440, #10071, #7883, .T. ) ;
#11876 = CARTESIAN_POINT ( 'NONE',  ( 6.207671477328696952, 3.321994320370140752, -4.246137054663666532 ) ) ;
#11877 = CARTESIAN_POINT ( 'NONE',  ( 0.000000000000000000, 0.000000000000000000, 0.000000000000000000 ) ) ;
#11878 = DIRECTION ( 'NONE',  ( -0.000000000000000000, -0.000000000000000000, -1.000000000000000000 ) ) ;
#11879 = ORIENTED_EDGE ( 'NONE', *, *, #302, .T. ) ;
#11880 = EDGE_CURVE ( 'NONE', #7285, #1218, #1233, .T. ) ;
#11881 = DIRECTION ( 'NONE',  ( 0.2873478855663427756, 0.9578262852211522071, 3.408579461568464094E-15 ) ) ;
#11882 = CARTESIAN_POINT ( 'NONE',  ( 0.2484800633749985332, 2.497823135841265252, -3.673643420401908166 ) ) ;
#11883 = DIRECTION ( 'NONE',  ( 1.000000000000000000, 0.000000000000000000, 0.000000000000000000 ) ) ;
#11885 = ADVANCED_FACE ( 'NONE', ( #1148 ), #252, .F. ) ;
#11884 = CARTESIAN_POINT ( 'NONE',  ( 701.6639754956653405, 161.3119797772417883, 177.6000000000001648 ) ) ;
#11886 = ORIENTED_EDGE ( 'NONE', *, *, #6239, .T. ) ;
#11887 = EDGE_LOOP ( 'NONE', ( #9606, #9176, #10003, #6507 ) ) ;
#11888 = PLANE ( 'NONE',  #10083 ) ;
#11889 = DIRECTION ( 'NONE',  ( -0.000000000000000000, -0.000000000000000000, 1.000000000000000000 ) ) ;
#11890 = CARTESIAN_POINT ( 'NONE',  ( 609.7124105659718225, 187.8865375995820557, -188.9268648956065419 ) ) ;
#11891 = CARTESIAN_POINT ( 'NONE',  ( 2.595115354961440524, -7.673029147243177306, -1.000000000000000000 ) ) ;
#11892 = ORIENTED_EDGE ( 'NONE', *, *, #427, .F. ) ;
#11893 = DIRECTION ( 'NONE',  ( 0.000000000000000000, 0.000000000000000000, 1.000000000000000000 ) ) ;
#11894 = CARTESIAN_POINT ( 'NONE',  ( 2.055025722542103583, 6.319083845363847374, -5.720331885005371042 ) ) ;
#11895 = CARTESIAN_POINT ( 'NONE',  ( -10.00000000000000000, 413.4403065089105667, -187.0000000000000000 ) ) ;
#11896 = CARTESIAN_POINT ( 'NONE',  ( 0.000000000000000000, 0.000000000000000000, 0.000000000000000000 ) ) ;
#11897 = FACE_OUTER_BOUND ( 'NONE', #2836, .T. ) ;
#11898 = CARTESIAN_POINT ( 'NONE',  ( 1.411581201560190495E-15, 4.862606272033091592, -3.745885042887436622 ) ) ;
#11899 = EDGE_LOOP ( 'NONE', ( #2376, #13706, #4592, #1438 ) ) ;
#11900 = CARTESIAN_POINT ( 'NONE',  ( 0.000000000000000000, 0.000000000000000000, 0.000000000000000000 ) ) ;
#11901 = ORIENTED_EDGE ( 'NONE', *, *, #6236, .T. ) ;
#11902 = ORIENTED_EDGE ( 'NONE', *, *, #13297, .T. ) ;
#11903 = LINE ( 'NONE', #4996, #5697 ) ;
#11904 = EDGE_CURVE ( 'NONE', #740, #9530, #4670, .T. ) ;
#11905 = LINE ( 'NONE', #8302, #13919 ) ;
#11906 = DIRECTION ( 'NONE',  ( -0.000000000000000000, -0.000000000000000000, 1.000000000000000000 ) ) ;
#11907 = ADVANCED_FACE ( 'NONE', ( #12659 ), #14595, .T. ) ;
#11908 = CARTESIAN_POINT ( 'NONE',  ( 470.8287951810180516, 310.9528939902474463, -190.0000000000000000 ) ) ;
#11909 = ORIENTED_EDGE ( 'NONE', *, *, #10399, .T. ) ;
#11910 = CARTESIAN_POINT ( 'NONE',  ( 6.357976367242104132, -3.426708043488309041, 4.282301071215474764 ) ) ;
#11911 = CARTESIAN_POINT ( 'NONE',  ( 642.5000000000001137, 160.9817477042468568, 210.0000119999999981 ) ) ;
#11912 = FACE_OUTER_BOUND ( 'NONE', #7818, .T. ) ;
#11913 = DIRECTION ( 'NONE',  ( -0.000000000000000000, -0.000000000000000000, -1.000000000000000000 ) ) ;
#11914 = VERTEX_POINT ( 'NONE', #13491 ) ;
#11915 = SURFACE_STYLE_FILL_AREA ( #14446 ) ;
#11916 = ORIENTED_EDGE ( 'NONE', *, *, #14089, .F. ) ;
#11917 = EDGE_CURVE ( 'NONE', #12598, #1859, #2253, .T. ) ;
#11918 = CARTESIAN_POINT ( 'NONE',  ( 641.0000000000000000, 154.0000000000000568, 187.5000000000000000 ) ) ;
#11919 = CARTESIAN_POINT ( 'NONE',  ( 228.5935732249376997, 306.3651924111334779, 182.7999999999996135 ) ) ;
#11920 = ORIENTED_EDGE ( 'NONE', *, *, #14317, .T. ) ;
#11921 = FACE_OUTER_BOUND ( 'NONE', #12585, .T. ) ;
#11922 = LINE ( 'NONE', #1817, #14139 ) ;
#11923 = CARTESIAN_POINT ( 'NONE',  ( -3.679171394226034675, -2.494631558665844739, -0.3503314178412558211 ) ) ;
#11924 = ORIENTED_EDGE ( 'NONE', *, *, #11880, .T. ) ;
#11925 = CARTESIAN_POINT ( 'NONE',  ( -4.000000000000000000, 2.511478553582031203, -3.469254451724764543 ) ) ;
#11926 = DIRECTION ( 'NONE',  ( 0.000000000000000000, 0.000000000000000000, 1.000000000000000000 ) ) ;
#11927 = ORIENTED_EDGE ( 'NONE', *, *, #10805, .T. ) ;
#11928 = EDGE_CURVE ( 'NONE', #11011, #8880, #3372, .T. ) ;
#11929 = ORIENTED_EDGE ( 'NONE', *, *, #6263, .F. ) ;
#11930 = VECTOR ( 'NONE', #109, 1000.000000000000000 ) ;
#11931 = CARTESIAN_POINT ( 'NONE',  ( 6.244297270354683960, 1.800816419761795034E-11, 5.105276777067893512 ) ) ;
#11932 = CARTESIAN_POINT ( 'NONE',  ( -9.999999999999998224, 376.8992337277234128, -187.0000000000000000 ) ) ;
#11933 = FACE_OUTER_BOUND ( 'NONE', #9561, .T. ) ;
#11934 = CIRCLE ( 'NONE', #10534, 3.399999999999999911 ) ;
#11935 = VECTOR ( 'NONE', #4710, 1000.000000000000000 ) ;
#11936 = PRODUCT ( 'stationary channel', 'stationary channel', '', ( #7755 ) ) ;
#11937 = CARTESIAN_POINT ( 'NONE',  ( -4.101948962586059899, -2.368261337751176754, -3.681124513963741851 ) ) ;
#11938 = MANIFOLD_SOLID_BREP ( 'Mirror13', #10452 ) ;
#11939 = UNCERTAINTY_MEASURE_WITH_UNIT (LENGTH_MEASURE( 1.000000000000000082E-05 ), #4163, 'distance_accuracy_value', 'NONE');
#11940 = CARTESIAN_POINT ( 'NONE',  ( 641.0000000000000000, 154.0000000000000568, 187.5000000000000000 ) ) ;
#11941 = ORIENTED_EDGE ( 'NONE', *, *, #12887, .F. ) ;
#11942 = DIRECTION ( 'NONE',  ( -1.000000000000000000, 0.000000000000000000, -0.000000000000000000 ) ) ;
#11943 = CARTESIAN_POINT ( 'NONE',  ( 635.0000000000000000, 160.0000000000000284, -210.0000000000000000 ) ) ;
#11944 = DIRECTION ( 'NONE',  ( 0.000000000000000000, 0.000000000000000000, -1.000000000000000000 ) ) ;
#11945 = ADVANCED_FACE ( 'NONE', ( #8092 ), #9058, .F. ) ;
#11946 = CIRCLE ( 'NONE', #8180, 5.750000000000000000 ) ;
#11947 = CARTESIAN_POINT ( 'NONE',  ( 112.9652219749295341, 376.5507399164317803, 210.0000000000000000 ) ) ;
#11948 = ORIENTED_EDGE ( 'NONE', *, *, #677, .F. ) ;
#11949 = VERTEX_POINT ( 'NONE', #13783 ) ;
#11950 = DIRECTION ( 'NONE',  ( 0.3543563944859322579, -0.9351104457158685435, 0.000000000000000000 ) ) ;
#11951 = DIRECTION ( 'NONE',  ( 0.2873478855663454401, 0.9578262852211514300, -3.831370512995697396E-15 ) ) ;
#11952 = ADVANCED_FACE ( 'NONE', ( #12438 ), #4633, .F. ) ;
#11953 = AXIS2_PLACEMENT_3D ( 'NONE', #8555, #8119, #13524 ) ;
#11954 = FACE_OUTER_BOUND ( 'NONE', #11575, .T. ) ;
#11955 = ADVANCED_FACE ( 'NONE', ( #10381 ), #8017, .T. ) ;
#11956 = EDGE_CURVE ( 'NONE', #5297, #931, #3671, .T. ) ;
#11957 = DIRECTION ( 'NONE',  ( 0.03086419753086420623, -0.9995235871707959241, 0.000000000000000000 ) ) ;
#11959 = VERTEX_POINT ( 'NONE', #11631 ) ;
#11958 = CIRCLE ( 'NONE', #12189, 8.331345277524542681 ) ;
#11960 = EDGE_CURVE ( 'NONE', #5405, #299, #6904, .T. ) ;
#11961 = TOROIDAL_SURFACE ( 'NONE', #5607, 2.700000000000000622, 0.2000000000000000111 ) ;
#11962 = CARTESIAN_POINT ( 'NONE',  ( 2.999999999999999112, -4.618802153516999631, 0.000000000000000000 ) ) ;
#11963 = CARTESIAN_POINT ( 'NONE',  ( 4.000000000000000000, 0.3987449864460005378, -0.01220643443059817035 ) ) ;
#11964 = DIRECTION ( 'NONE',  ( 0.9578262852211513190, -0.2873478855663454956, 0.000000000000000000 ) ) ;
#11965 = ORIENTED_EDGE ( 'NONE', *, *, #11668, .F. ) ;
#11966 = CARTESIAN_POINT ( 'NONE',  ( 2.999999999999999112, 0.000000000000000000, 0.000000000000000000 ) ) ;
#11967 = CARTESIAN_POINT ( 'NONE',  ( 4.799999999999999822, 0.000000000000000000, 0.000000000000000000 ) ) ;
#11968 = LINE ( 'NONE', #12182, #4213 ) ;
#11969 = ORIENTED_EDGE ( 'NONE', *, *, #13987, .T. ) ;
#11970 = CARTESIAN_POINT ( 'NONE',  ( -111.4713065522750952, 33.44139196568231398, -190.0000000000000000 ) ) ;
#11971 = MANIFOLD_SOLID_BREP ( 'Mirror2', #7391 ) ;
#11972 = ORIENTED_EDGE ( 'NONE', *, *, #1375, .F. ) ;
#11973 = ORIENTED_EDGE ( 'NONE', *, *, #9376, .F. ) ;
#11974 = DIRECTION ( 'NONE',  ( 1.000000000000000000, 0.000000000000000000, 0.000000000000000000 ) ) ;
#11975 = AXIS2_PLACEMENT_3D ( 'NONE', #5590, #11201, #8700 ) ;
#11976 = CIRCLE ( 'NONE', #3270, 4.199999999999981526 ) ;
#11977 = AXIS2_PLACEMENT_3D ( 'NONE', #1410, #2509, #12562 ) ;
#11978 = ADVANCED_FACE ( 'NONE', ( #14010 ), #5141, .F. ) ;
#11979 = EDGE_CURVE ( 'NONE', #5936, #2950, #8381, .T. ) ;
#11980 = DIRECTION ( 'NONE',  ( 0.000000000000000000, 0.000000000000000000, -1.000000000000000000 ) ) ;
#11981 = ORIENTED_EDGE ( 'NONE', *, *, #6531, .T. ) ;
#11982 = ORIENTED_EDGE ( 'NONE', *, *, #1273, .F. ) ;
#11983 = DIRECTION ( 'NONE',  ( 0.000000000000000000, 0.000000000000000000, -1.000000000000000000 ) ) ;
#11984 = FACE_OUTER_BOUND ( 'NONE', #4653, .T. ) ;
#11985 = CIRCLE ( 'NONE', #9170, 2.649999999999985700 ) ;
#11986 = AXIS2_PLACEMENT_3D ( 'NONE', #10560, #8191, #12702 ) ;
#11987 = CARTESIAN_POINT ( 'NONE',  ( 470.8287951810180516, 310.9528939902474463, 190.0000000000000000 ) ) ;
#11988 = CARTESIAN_POINT ( 'NONE',  ( 635.0000000000000000, 160.0000000000000284, 211.0000000000000000 ) ) ;
#11989 = ORIENTED_EDGE ( 'NONE', *, *, #8930, .F. ) ;
#11990 = ADVANCED_FACE ( 'NONE', ( #12819 ), #2551, .F. ) ;
#11991 = CARTESIAN_POINT ( 'NONE',  ( 609.9372209285376130, 185.6979141947072378, 185.1431837845556743 ) ) ;
#11992 = DIRECTION ( 'NONE',  ( 0.000000000000000000, 1.000000000000000000, 0.000000000000000000 ) ) ;
#11993 = VERTEX_POINT ( 'NONE', #320 ) ;
#11994 = DIRECTION ( 'NONE',  ( 0.2873478855663454401, 0.9578262852211514300, -3.927332483172771155E-15 ) ) ;
#11995=STYLED_ITEM('',(#14681),#7073);
#11996 = VERTEX_POINT ( 'NONE', #7136 ) ;
#11997 = VECTOR ( 'NONE', #5827, 1000.000000000000000 ) ;
#11998 = AXIS2_PLACEMENT_3D ( 'NONE', #6331, #7729, #7591 ) ;
#11999 = CARTESIAN_POINT ( 'NONE',  ( 148.9991633467111569, 386.6211705227183870, 210.0000000000000000 ) ) ;
#12000 = CARTESIAN_POINT ( 'NONE',  ( 148.9991633467111569, 386.6211705227183870, -210.0000000000000000 ) ) ;
#12001 = ORIENTED_EDGE ( 'NONE', *, *, #4356, .T. ) ;
#12002 = CARTESIAN_POINT ( 'NONE',  ( 228.5935732249376997, 306.3651924111334779, 179.7999999999995850 ) ) ;
#12003 = DIRECTION ( 'NONE',  ( 0.000000000000000000, 0.000000000000000000, 1.000000000000000000 ) ) ;
#12004 = VECTOR ( 'NONE', #14598, 1000.000000000000000 ) ;
#12005 = FACE_BOUND ( 'NONE', #14140, .T. ) ;
#12006 =( NAMED_UNIT ( * ) SI_UNIT ( $, .STERADIAN. ) SOLID_ANGLE_UNIT ( ) );
#12007 = ORIENTED_EDGE ( 'NONE', *, *, #3637, .T. ) ;
#12008 = CIRCLE ( 'NONE', #3307, 0.7500000000000000000 ) ;
#12009 = AXIS2_PLACEMENT_3D ( 'NONE', #8360, #12866, #9401 ) ;
#12010 = CARTESIAN_POINT ( 'NONE',  ( 6.244889965166094292, 3.924082311521017274, 3.413878157001050795 ) ) ;
#12011 = ORIENTED_EDGE ( 'NONE', *, *, #6113, .T. ) ;
#12012 = ORIENTED_EDGE ( 'NONE', *, *, #3062, .F. ) ;
#12013 = VECTOR ( 'NONE', #12636, 1000.000000000000000 ) ;
#12014 = AXIS2_PLACEMENT_3D ( 'NONE', #2311, #10291, #5858 ) ;
#12015 = DIRECTION ( 'NONE',  ( 1.000000000000000000, 0.000000000000000000, 0.000000000000000000 ) ) ;
#12017 = CIRCLE ( 'NONE', #7799, 6.080745460913608902 ) ;
#12016 = CARTESIAN_POINT ( 'NONE',  ( 4.000000000000000000, 0.000000000000000000, -25.03750572909317285 ) ) ;
#12018 = AXIS2_PLACEMENT_3D ( 'NONE', #3724, #2688, #8208 ) ;
#12019 = ADVANCED_FACE ( 'NONE', ( #2772, #6245 ), #1671, .T. ) ;
#12020 = CARTESIAN_POINT ( 'NONE',  ( 2.999999999999999112, 4.618802153517012954, 0.000000000000000000 ) ) ;
#12021 = VECTOR ( 'NONE', #1034, 1000.000000000000000 ) ;
#12022 = CARTESIAN_POINT ( 'NONE',  ( -9.511508594537124495, 378.5275384125996538, 187.0000000000000284 ) ) ;
#12023 = ORIENTED_EDGE ( 'NONE', *, *, #5317, .T. ) ;
#12024 = VECTOR ( 'NONE', #1993, 1000.000000000000114 ) ;
#12025 = CARTESIAN_POINT ( 'NONE',  ( 6.196878017913833858, -1.924500897298760727, -5.000000000000000888 ) ) ;
#12026 = DIRECTION ( 'NONE',  ( -0.000000000000000000, -0.000000000000000000, -1.000000000000000000 ) ) ;
#12027 = SHAPE_DEFINITION_REPRESENTATION ( #5807, #6779 ) ;
#12028 = VECTOR ( 'NONE', #2711, 1000.000000000000000 ) ;
#12029 = CARTESIAN_POINT ( 'NONE',  ( 148.9991633467111569, 386.6211705227183870, -190.0000000000000568 ) ) ;
#12030 = EDGE_LOOP ( 'NONE', ( #12440, #9127, #10646, #4373 ) ) ;
#12031 = VERTEX_POINT ( 'NONE', #13933 ) ;
#12032 = DIRECTION ( 'NONE',  ( 1.000000000000000000, 0.000000000000000000, 0.000000000000000000 ) ) ;
#12033 = CARTESIAN_POINT ( 'NONE',  ( 102.3333502089745650, 341.1111673632485122, -1.352973838917536986E-12 ) ) ;
#12034 = DIRECTION ( 'NONE',  ( -2.449021377849607626E-15, -3.265361837132810036E-15, 1.000000000000000000 ) ) ;
#12035 = VECTOR ( 'NONE', #13423, 999.9999999999998863 ) ;
#12036 = AXIS2_PLACEMENT_3D ( 'NONE', #14579, #10294, #5645 ) ;
#12037 = EDGE_CURVE ( 'NONE', #2553, #6810, #9643, .T. ) ;
#12038 = CARTESIAN_POINT ( 'NONE',  ( 6.500000000000002665, 2.501851166488374911, -5.848636054922036642 ) ) ;
#12039 = CIRCLE ( 'NONE', #5460, 6.080745460913608902 ) ;
#12040 = ORIENTED_EDGE ( 'NONE', *, *, #10385, .T. ) ;
#12041 = CARTESIAN_POINT ( 'NONE',  ( -6.500000000000000888, 2.759383090082417667, -5.880088986491048608 ) ) ;
#12042 = ORIENTED_EDGE ( 'NONE', *, *, #10626, .F. ) ;
#12043 = ADVANCED_FACE ( 'NONE', ( #5077 ), #9572, .F. ) ;
#12044 = CARTESIAN_POINT ( 'NONE',  ( 610.0000000000000000, 0.000000000000000000, 210.0000000000000000 ) ) ;
#12045 = FACE_OUTER_BOUND ( 'NONE', #13245, .T. ) ;
#12046 = DIRECTION ( 'NONE',  ( 0.000000000000000000, -0.5000000000000009992, -0.8660254037844380415 ) ) ;
#12047 = VECTOR ( 'NONE', #3164, 1000.000000000000227 ) ;
#12048 = VERTEX_POINT ( 'NONE', #12962 ) ;
#12049 = VECTOR ( 'NONE', #3817, 1000.000000000000000 ) ;
#12050 = ADVANCED_FACE ( 'NONE', ( #10744 ), #2852, .F. ) ;
#12051 = CARTESIAN_POINT ( 'NONE',  ( 0.3572655899081558228, -2.309401076758485161, 3.999999999999999112 ) ) ;
#12052 = EDGE_LOOP ( 'NONE', ( #5360, #12128, #13893, #7478 ) ) ;
#12053 = EDGE_LOOP ( 'NONE', ( #12990, #6749, #5427, #10426, #8610, #9698 ) ) ;
#12054 = EDGE_CURVE ( 'NONE', #6460, #12082, #1712, .T. ) ;
#12055 = CARTESIAN_POINT ( 'NONE',  ( 0.3106000600989257121, 3.122278952918442485, -4.592054218142294530 ) ) ;
#12056 = EDGE_CURVE ( 'NONE', #11914, #9303, #5959, .T. ) ;
#12057 =( GEOMETRIC_REPRESENTATION_CONTEXT ( 3 ) GLOBAL_UNCERTAINTY_ASSIGNED_CONTEXT ( ( #13885 ) ) GLOBAL_UNIT_ASSIGNED_CONTEXT ( ( #12645, #5941, #10442 ) ) REPRESENTATION_CONTEXT ( 'NONE', 'WORKASPACE' ) );
#12058 = CARTESIAN_POINT ( 'NONE',  ( 10.00000000000000000, 0.000000000000000000, 210.0000000000000000 ) ) ;
#12059 = AXIS2_PLACEMENT_3D ( 'NONE', #14053, #4904, #3654 ) ;
#12060 = EDGE_LOOP ( 'NONE', ( #5326, #84, #11416, #9004 ) ) ;
#12061 = ORIENTED_EDGE ( 'NONE', *, *, #9065, .T. ) ;
#12062 = LINE ( 'NONE', #10814, #7113 ) ;
#12063 =( REPRESENTATION_RELATIONSHIP ('NONE','NONE', #2822, #1780 ) REPRESENTATION_RELATIONSHIP_WITH_TRANSFORMATION ( #9791 )SHAPE_REPRESENTATION_RELATIONSHIP( ) );
#12064 = CARTESIAN_POINT ( 'NONE',  ( 633.0368908673054875, 167.3047950750124642, 210.0000119999999981 ) ) ;
#12065 = DIRECTION ( 'NONE',  ( -0.000000000000000000, -0.000000000000000000, 1.000000000000000000 ) ) ;
#12066 = DIRECTION ( 'NONE',  ( 0.000000000000000000, 0.000000000000000000, 1.000000000000000000 ) ) ;
#12067 =( LENGTH_UNIT ( ) NAMED_UNIT ( * ) SI_UNIT ( .MILLI., .METRE. ) );
#12068 = ORIENTED_EDGE ( 'NONE', *, *, #8000, .F. ) ;
#12069 = EDGE_CURVE ( 'NONE', #9255, #10781, #13179, .T. ) ;
#12070 = DIRECTION ( 'NONE',  ( -0.9578262852211508749, 0.2873478855663467724, -0.000000000000000000 ) ) ;
#12071 = FACE_OUTER_BOUND ( 'NONE', #13266, .T. ) ;
#12072 = ITEM_DEFINED_TRANSFORMATION ( 'NONE', 'NONE', #11834,  #9440 ) ;
#12073 = ORIENTED_EDGE ( 'NONE', *, *, #10443, .T. ) ;
#12074 = AXIS2_PLACEMENT_3D ( 'NONE', #11640, #2787, #6117 ) ;
#12075 = CARTESIAN_POINT ( 'NONE',  ( 102.3333502089745934, 341.1111673632486259, -1.398642936228627705E-12 ) ) ;
#12076 = EDGE_CURVE ( 'NONE', #13752, #10951, #14361, .T. ) ;
#12077 = EDGE_LOOP ( 'NONE', ( #12892, #6558, #7632 ) ) ;
#12078 = PRODUCT_DEFINITION_FORMATION_WITH_SPECIFIED_SOURCE ( 'ANY', '', #6049, .NOT_KNOWN. ) ;
#12079 = LINE ( 'NONE', #5576, #12476 ) ;
#12080 = DIRECTION ( 'NONE',  ( -1.000000000000000000, 0.000000000000000000, 0.000000000000000000 ) ) ;
#12081 = MECHANICAL_DESIGN_GEOMETRIC_PRESENTATION_REPRESENTATION (  '', ( #2898 ), #7366 ) ;
#12082 = VERTEX_POINT ( 'NONE', #5508 ) ;
#12083 = DIRECTION ( 'NONE',  ( 0.000000000000000000, 0.000000000000000000, 1.000000000000000000 ) ) ;
#12084 = FACE_OUTER_BOUND ( 'NONE', #5822, .T. ) ;
#12085 = CARTESIAN_POINT ( 'NONE',  ( 630.5661054975340676, 158.1613647612965110, 210.0000000000000000 ) ) ;
#12086 = ORIENTED_EDGE ( 'NONE', *, *, #966, .T. ) ;
#12087 = DIRECTION ( 'NONE',  ( 1.063400795443704616E-15, -3.190202386331113848E-16, -1.000000000000000000 ) ) ;
#12088 = CARTESIAN_POINT ( 'NONE',  ( 2.000000000000000000, -6.429618962271402616, -1.000000000000000000 ) ) ;
#12089 = ORIENTED_EDGE ( 'NONE', *, *, #14580, .F. ) ;
#12090 = ORIENTED_EDGE ( 'NONE', *, *, #11063, .F. ) ;
#12091 = VECTOR ( 'NONE', #11537, 1000.000000000000000 ) ;
#12092 = CARTESIAN_POINT ( 'NONE',  ( 0.000000000000000000, 5.258101095580073669E-15, 4.000000000000000000 ) ) ;
#12093 = VECTOR ( 'NONE', #8288, 1000.000000000000000 ) ;
#12094 = DIRECTION ( 'NONE',  ( -0.000000000000000000, -0.000000000000000000, 1.000000000000000000 ) ) ;
#12095 = CARTESIAN_POINT ( 'NONE',  ( 6.362374563308399900, 5.433808049140282037, -0.8060918076007316246 ) ) ;
#12096 = CARTESIAN_POINT ( 'NONE',  ( 10.00000000000000000, -10.00000000000000000, -210.0020000000000095 ) ) ;
#12097 = ADVANCED_FACE ( 'NONE', ( #8758 ), #10680, .T. ) ;
#12098 = DIRECTION ( 'NONE',  ( 0.9578262852211489875, -0.2873478855663534892, 0.000000000000000000 ) ) ;
#12099 = ORIENTED_EDGE ( 'NONE', *, *, #6106, .T. ) ;
#12100 = LINE ( 'NONE', #2052, #13170 ) ;
#12101 = DIRECTION ( 'NONE',  ( -0.2873478855663470499, -0.9578262852211508749, -0.000000000000000000 ) ) ;
#12102 = DIRECTION ( 'NONE',  ( -1.000000000000000000, 0.000000000000000000, 0.000000000000000000 ) ) ;
#12103 = CARTESIAN_POINT ( 'NONE',  ( 6.367873360227555679, -2.886751345948120662, 4.999999999999999112 ) ) ;
#12104 = VERTEX_POINT ( 'NONE', #11109 ) ;
#12105 = ORIENTED_EDGE ( 'NONE', *, *, #7397, .T. ) ;
#12106 = DIRECTION ( 'NONE',  ( -0.000000000000000000, -0.000000000000000000, 1.000000000000000000 ) ) ;
#12107 = DIRECTION ( 'NONE',  ( -1.000000000000000000, 0.000000000000000000, 0.000000000000000000 ) ) ;
#12108 = ADVANCED_FACE ( 'NONE', ( #9853 ), #991, .T. ) ;
#12109 = EDGE_CURVE ( 'NONE', #14129, #10035, #5485, .T. ) ;
#12110 = FACE_OUTER_BOUND ( 'NONE', #1095, .T. ) ;
#12111 = LINE ( 'NONE', #13152, #233 ) ;
#12112 = VERTEX_POINT ( 'NONE', #13108 ) ;
#12113 = FACE_OUTER_BOUND ( 'NONE', #11607, .T. ) ;
#12114 = VERTEX_POINT ( 'NONE', #4175 ) ;
#12115 = DIRECTION ( 'NONE',  ( -1.000000000000000000, 0.000000000000000000, 0.000000000000000000 ) ) ;
#12116 = CARTESIAN_POINT ( 'NONE',  ( 3.383466608491643077E-15, 4.736522675502341073, -3.681124513963742739 ) ) ;
#12117 = DIRECTION ( 'NONE',  ( -1.000000000000000000, 0.000000000000000000, 0.000000000000000000 ) ) ;
#12118 =( LENGTH_UNIT ( ) NAMED_UNIT ( * ) SI_UNIT ( .MILLI., .METRE. ) );
#12119 = ORIENTED_EDGE ( 'NONE', *, *, #6301, .T. ) ;
#12120 = CARTESIAN_POINT ( 'NONE',  ( 708.1388811837590538, 164.7984674554467404, 177.5999999999999091 ) ) ;
#12121 = EDGE_LOOP ( 'NONE', ( #3591, #11081 ) ) ;
#12122 = ORIENTED_EDGE ( 'NONE', *, *, #10090, .F. ) ;
#12123 = CARTESIAN_POINT ( 'NONE',  ( 635.0000000000000000, 160.0000000000000284, -207.0000000000000000 ) ) ;
#12124 = ADVANCED_FACE ( 'NONE', ( #10899 ), #10449, .T. ) ;
#12125 = DIRECTION ( 'NONE',  ( 9.794481010665704304E-16, 3.264827003555233190E-15, 1.000000000000000000 ) ) ;
#12126 = DIRECTION ( 'NONE',  ( -0.000000000000000000, 1.000000000000000000, 1.224646799147353207E-16 ) ) ;
#12127 =( BOUNDED_SURFACE ( )  B_SPLINE_SURFACE ( 3, 2, ( 
 ( #10366, #307, #13832 ),
 ( #12945, #2755, #7192 ),
 ( #13997, #4843, #8215 ),
 ( #9336, #1511, #2835 ),
 ( #7338, #1653, #3885 ),
 ( #10507, #13767, #10584 ) ),
 .UNSPECIFIED., .F., .F., .T. ) 
 B_SPLINE_SURFACE_WITH_KNOTS ( ( 4, 2, 4 ),
 ( 3, 3 ),
 ( 0.02032853247518126918, 0.02278863295364821906, 0.02524873343211517240 ),
 ( 0.000000000000000000, 1.000000000000000000 ),
 .UNSPECIFIED. ) 
 GEOMETRIC_REPRESENTATION_ITEM ( )  RATIONAL_B_SPLINE_SURFACE ( (
 ( 1.000000000000000000, 0.8047781615896837382, 1.000000000000000000),
 ( 1.000000000000000000, 0.8123767586289252218, 1.000000000000000000),
 ( 1.000000000000000000, 0.8190662415564388121, 1.000000000000000000),
 ( 1.000000000000000000, 0.8192361015669026303, 1.000000000000000000),
 ( 1.000000000000000000, 0.8126135807103900266, 1.000000000000000000),
 ( 1.000000000000000000, 0.8047712338318593339, 1.000000000000000000) ) ) 
 REPRESENTATION_ITEM ( '' )  SURFACE ( )  );
#12129 = EDGE_CURVE ( 'NONE', #14483, #7000, #12320, .T. ) ;
#12128 = ORIENTED_EDGE ( 'NONE', *, *, #9982, .F. ) ;
#12130 = ORIENTED_EDGE ( 'NONE', *, *, #3460, .F. ) ;
#12131 = CARTESIAN_POINT ( 'NONE',  ( 6.242800618755127928, -3.923709308887747937, 3.414402460853335874 ) ) ;
#12132 = CARTESIAN_POINT ( 'NONE',  ( 0.000000000000000000, 3.061616997868383634E-16, -2.500000000000000444 ) ) ;
#12133 = LINE ( 'NONE', #14169, #2783 ) ;
#12134 = CARTESIAN_POINT ( 'NONE',  ( 139.8040310085880833, 355.9707293956415697, -210.0000000000000000 ) ) ;
#12135 = DIRECTION ( 'NONE',  ( -0.000000000000000000, 0.000000000000000000, -1.000000000000000000 ) ) ;
#12136 = FILL_AREA_STYLE ('',( #14223 ) ) ;
#12137 = EDGE_LOOP ( 'NONE', ( #5279, #5454, #14493, #5321 ) ) ;
#12138 = CARTESIAN_POINT ( 'NONE',  ( -6.080745460913608902, 0.5192545390863924082, 0.000000000000000000 ) ) ;
#12139 = ADVANCED_FACE ( 'NONE', ( #6609, #12198 ), #5433, .T. ) ;
#12140 = ORIENTED_EDGE ( 'NONE', *, *, #14136, .F. ) ;
#12141 = LINE ( 'NONE', #8890, #3813 ) ;
#12142 = EDGE_CURVE ( 'NONE', #11914, #6340, #7653, .T. ) ;
#12143 = EDGE_LOOP ( 'NONE', ( #954, #4106, #13538, #12546 ) ) ;
#12144 = CARTESIAN_POINT ( 'NONE',  ( 631.0000000000000000, 164.0000000000000284, -233.5000000000000000 ) ) ;
#12145 = EDGE_CURVE ( 'NONE', #2108, #10293, #5497, .T. ) ;
#12146 = LINE ( 'NONE', #2030, #8761 ) ;
#12147 = ADVANCED_FACE ( 'NONE', ( #11028 ), #7860, .T. ) ;
#12148 = ORIENTED_EDGE ( 'NONE', *, *, #7283, .T. ) ;
#12149 = CARTESIAN_POINT ( 'NONE',  ( -8.505790995055066972, 376.6597771564184427, 187.0000000000000284 ) ) ;
#12150 = DIRECTION ( 'NONE',  ( 1.000000000000000000, 0.000000000000000000, 0.000000000000000000 ) ) ;
#12151 = EDGE_CURVE ( 'NONE', #12303, #13614, #2185, .T. ) ;
#12152 = CARTESIAN_POINT ( 'NONE',  ( -10.00000000000003730, 371.6790804732684137, 169.9999999999999716 ) ) ;
#12153 = VERTEX_POINT ( 'NONE', #14288 ) ;
#12154 = LINE ( 'NONE', #4195, #5864 ) ;
#12155 = VERTEX_POINT ( 'NONE', #13322 ) ;
#12156 = EDGE_LOOP ( 'NONE', ( #10690, #4219, #4086, #224 ) ) ;
#12157 = CARTESIAN_POINT ( 'NONE',  ( 2.055025722541879318, -6.319083845363985930, -5.720331885005374595 ) ) ;
#12158 = CARTESIAN_POINT ( 'NONE',  ( 610.0000000000002274, 185.6790804732683284, 169.9999999999999716 ) ) ;
#12159 = ADVANCED_FACE ( 'NONE', ( #4393 ), #6535, .F. ) ;
#12160 = CARTESIAN_POINT ( 'NONE',  ( 610.8620436566991430, 188.5525593289318920, 187.0000000000000000 ) ) ;
#12161 = DIRECTION ( 'NONE',  ( -1.000000000000000000, 0.000000000000000000, 0.000000000000000000 ) ) ;
#12162 = CYLINDRICAL_SURFACE ( 'NONE', #2272, 4.799999999999968736 ) ;
#12163 = VERTEX_POINT ( 'NONE', #10819 ) ;
#12164 = LINE ( 'NONE', #9891, #2760 ) ;
#12165 = CARTESIAN_POINT ( 'NONE',  ( 0.000000000000000000, 0.000000000000000000, 0.000000000000000000 ) ) ;
#12166 = CONTEXT_DEPENDENT_SHAPE_REPRESENTATION ( #12623, #10527 ) ;
#12167 = CARTESIAN_POINT ( 'NONE',  ( 148.9991633467111569, 386.6211705227183870, -190.0000000000000568 ) ) ;
#12168 = ADVANCED_FACE ( 'NONE', ( #7713 ), #8673, .F. ) ;
#12169 = ORIENTED_EDGE ( 'NONE', *, *, #5865, .F. ) ;
#12170 = ORIENTED_EDGE ( 'NONE', *, *, #3737, .T. ) ;
#12171 = SURFACE_STYLE_USAGE ( .BOTH. , #13294 ) ;
#12172 = CARTESIAN_POINT ( 'NONE',  ( -5.978033218201117549, -4.054134411712201569, -0.5602453477493345435 ) ) ;
#12173 = EDGE_CURVE ( 'NONE', #1912, #13547, #1961, .T. ) ;
#12174 = DIRECTION ( 'NONE',  ( 0.000000000000000000, 0.000000000000000000, 1.000000000000000000 ) ) ;
#12175 = CARTESIAN_POINT ( 'NONE',  ( 2.262848203703083261, 6.566616684922145453, -6.208169345099790348 ) ) ;
#12176 = VERTEX_POINT ( 'NONE', #5786 ) ;
#12177 = CARTESIAN_POINT ( 'NONE',  ( -6.499999999999424460, 2.723853875611551789, -6.224027332484248554 ) ) ;
#12178 = ORIENTED_EDGE ( 'NONE', *, *, #9510, .F. ) ;
#12179 = CIRCLE ( 'NONE', #5593, 4.000000000000000000 ) ;
#12180 = DIRECTION ( 'NONE',  ( 0.000000000000000000, 0.000000000000000000, -1.000000000000000000 ) ) ;
#12181 = CYLINDRICAL_SURFACE ( 'NONE', #670, 2.100000000000000089 ) ;
#12182 = CARTESIAN_POINT ( 'NONE',  ( 3.309651814758565180, -5.455921364805393026, 0.000000000000000000 ) ) ;
#12183 = ORIENTED_EDGE ( 'NONE', *, *, #8403, .F. ) ;
#12184 = DIRECTION ( 'NONE',  ( -1.000000000000000000, 0.000000000000000000, 0.000000000000000000 ) ) ;
#12185 = ORIENTED_EDGE ( 'NONE', *, *, #10706, .T. ) ;
#12186 = ORIENTED_EDGE ( 'NONE', *, *, #6557, .F. ) ;
#12187 = LINE ( 'NONE', #13248, #3821 ) ;
#12188 = CARTESIAN_POINT ( 'NONE',  ( 33.50000000000000000, 0.000000000000000000, 0.000000000000000000 ) ) ;
#12189 = AXIS2_PLACEMENT_3D ( 'NONE', #2139, #3337, #7841 ) ;
#12190 = CARTESIAN_POINT ( 'NONE',  ( 4.000000000000000000, -2.511475576507276042, -3.469253905236643565 ) ) ;
#12191 = ORIENTED_EDGE ( 'NONE', *, *, #10333, .F. ) ;
#12192 = VERTEX_POINT ( 'NONE', #11461 ) ;
#12193 = CARTESIAN_POINT ( 'NONE',  ( 635.0000000000000000, 160.0000000000000284, -207.0000000000000000 ) ) ;
#12194 = EDGE_CURVE ( 'NONE', #12510, #6357, #3284, .T. ) ;
#12195 = DIRECTION ( 'NONE',  ( 0.000000000000000000, 0.000000000000000000, 1.000000000000000000 ) ) ;
#12196 = LINE ( 'NONE', #2089, #5379 ) ;
#12197 = DIRECTION ( 'NONE',  ( 1.063400795443704616E-15, -3.190202386331113848E-16, -1.000000000000000000 ) ) ;
#12198 = FACE_OUTER_BOUND ( 'NONE', #7864, .T. ) ;
#12199 = ORIENTED_EDGE ( 'NONE', *, *, #5984, .T. ) ;
#12200 = LINE ( 'NONE', #14363, #8234 ) ;
#12201 = CIRCLE ( 'NONE', #13394, 7.500000000000062172 ) ;
#12202 = ORIENTED_EDGE ( 'NONE', *, *, #12503, .T. ) ;
#12203 = DIRECTION ( 'NONE',  ( -0.2873478855663453846, -0.9578262852211513190, 0.000000000000000000 ) ) ;
#12204 = ORIENTED_EDGE ( 'NONE', *, *, #222, .F. ) ;
#12205 = CARTESIAN_POINT ( 'NONE',  ( 8.500000000000000000, -5.773502691896264416, 0.000000000000000000 ) ) ;
#12206 = CARTESIAN_POINT ( 'NONE',  ( 0.5590169943749478954, 8.266365894244635319E-16, -6.750000000000000000 ) ) ;
#12207 = CIRCLE ( 'NONE', #1141, 5.200000000000004619 ) ;
#12208 = CIRCLE ( 'NONE', #5859, 4.799999999999968736 ) ;
#12209 = VERTEX_POINT ( 'NONE', #12498 ) ;
#12210 = CARTESIAN_POINT ( 'NONE',  ( 7.336184427528458230, 0.000000000000000000, 0.000000000000000000 ) ) ;
#12211 = ADVANCED_FACE ( 'NONE', ( #3588 ), #5566, .F. ) ;
#12212 = LINE ( 'NONE', #13272, #12957 ) ;
#12213 = FACE_OUTER_BOUND ( 'NONE', #2708, .T. ) ;
#12214 =( NAMED_UNIT ( * ) PLANE_ANGLE_UNIT ( ) SI_UNIT ( $, .RADIAN. ) );
#12215 = EDGE_LOOP ( 'NONE', ( #12422, #8003, #9140, #9184 ) ) ;
#12216 = EDGE_CURVE ( 'NONE', #13752, #1456, #11323, .T. ) ;
#12217 = FILL_AREA_STYLE ('',( #13340 ) ) ;
#12218 = EDGE_LOOP ( 'NONE', ( #14418, #3614, #13759, #11901 ) ) ;
#12219 = AXIS2_PLACEMENT_3D ( 'NONE', #10431, #7106, #4899 ) ;
#12220 = EDGE_CURVE ( 'NONE', #1327, #4881, #11171, .T. ) ;
#12221 = VECTOR ( 'NONE', #10775, 1000.000000000000114 ) ;
#12222 = ORIENTED_EDGE ( 'NONE', *, *, #3492, .F. ) ;
#12223 = DIRECTION ( 'NONE',  ( 0.000000000000000000, 0.000000000000000000, 1.000000000000000000 ) ) ;
#12224 = ADVANCED_FACE ( 'NONE', ( #5720 ), #13544, .T. ) ;
#12225 = CARTESIAN_POINT ( 'NONE',  ( 2.500000000000000000, 0.000000000000000000, 0.000000000000000000 ) ) ;
#12226 = CIRCLE ( 'NONE', #7534, 0.7500000000000000000 ) ;
#12227 = B_SPLINE_CURVE_WITH_KNOTS ( 'NONE', 3,
 ( #477, #2636, #316, #5006, #14007, #13929, #2848, #4854 ),
 .UNSPECIFIED., .F., .F.,
 ( 4, 2, 2, 4 ),
 ( 7.780516681398759253E-20, 0.002450665683189819696, 0.003675998524784729327, 0.004901331366379639391 ),
 .UNSPECIFIED. ) ;
#12228 = CARTESIAN_POINT ( 'NONE',  ( 0.000000000000000000, 0.000000000000000000, 0.000000000000000000 ) ) ;
#12229 = CYLINDRICAL_SURFACE ( 'NONE', #10158, 4.199999999999981526 ) ;
#12230 = VECTOR ( 'NONE', #10115, 1000.000000000000227 ) ;
#12231 = AXIS2_PLACEMENT_3D ( 'NONE', #8984, #3442, #6758 ) ;
#12232 = CARTESIAN_POINT ( 'NONE',  ( 0.03458865240850033523, 0.7871057074736559356, -4.000000000000000000 ) ) ;
#12233 = DIRECTION ( 'NONE',  ( 1.000000000000000000, 0.000000000000000000, -0.000000000000000000 ) ) ;
#12234 = PLANE ( 'NONE',  #10245 ) ;
#12235 = ORIENTED_EDGE ( 'NONE', *, *, #1048, .T. ) ;
#12236 = DIRECTION ( 'NONE',  ( 0.2873478855663446629, 0.9578262852211516520, 2.259726690317875391E-15 ) ) ;
#12237 = CARTESIAN_POINT ( 'NONE',  ( 0.000000000000000000, 0.000000000000000000, 0.000000000000000000 ) ) ;
#12238 = SHAPE_DEFINITION_REPRESENTATION ( #2505, #2248 ) ;
#12240 = EDGE_CURVE ( 'NONE', #3170, #5923, #6820, .T. ) ;
#12239 = AXIS2_PLACEMENT_3D ( 'NONE', #1216, #5722, #12282 ) ;
#12241 = EDGE_CURVE ( 'NONE', #5634, #8790, #4619, .T. ) ;
#12242 = CARTESIAN_POINT ( 'NONE',  ( -1.500000000000001332, 0.000000000000000000, 0.000000000000000000 ) ) ;
#12243 = ORIENTED_EDGE ( 'NONE', *, *, #2228, .F. ) ;
#12244 = ORIENTED_EDGE ( 'NONE', *, *, #10461, .T. ) ;
#12245 = SURFACE_STYLE_USAGE ( .BOTH. , #9897 ) ;
#12246 = LINE ( 'NONE', #3553, #8967 ) ;
#12247 = CIRCLE ( 'NONE', #8245, 5.000000000000000000 ) ;
#12248 = EDGE_CURVE ( 'NONE', #4518, #796, #1127, .T. ) ;
#12249 = AXIS2_PLACEMENT_3D ( 'NONE', #5217, #1740, #5289 ) ;
#12250 = PLANE ( 'NONE',  #6592 ) ;
#12251 = VECTOR ( 'NONE', #6443, 1000.000000000000000 ) ;
#12252 = CARTESIAN_POINT ( 'NONE',  ( 6.500000000000000000, 3.752776749732563921, -6.064240316920399110 ) ) ;
#12253 = VECTOR ( 'NONE', #12632, 1000.000000000000000 ) ;
#12254 = VERTEX_POINT ( 'NONE', #4692 ) ;
#12255 = DIRECTION ( 'NONE',  ( 0.000000000000000000, 0.000000000000000000, 1.000000000000000000 ) ) ;
#12256 = EDGE_LOOP ( 'NONE', ( #969, #10324, #12882, #12748 ) ) ;
#12257 = AXIS2_PLACEMENT_3D ( 'NONE', #13380, #3143, #4384 ) ;
#12258 = DIRECTION ( 'NONE',  ( 9.794481010665704304E-16, 3.264827003555234768E-15, -1.000000000000000000 ) ) ;
#12259 = CARTESIAN_POINT ( 'NONE',  ( 148.9991633467111569, 386.6211705227183870, 190.0000000000000568 ) ) ;
#12260 = DIRECTION ( 'NONE',  ( -0.4113766427172328433, 0.9114654452181377708, 0.000000000000000000 ) ) ;
#12261 = B_SPLINE_CURVE_WITH_KNOTS ( 'NONE', 3,
 ( #13730, #8107, #7291, #8393, #3843, #7152 ),
 .UNSPECIFIED., .F., .F.,
 ( 4, 2, 4 ),
 ( -4.604908129291797664E-06, 0.0003318387708540428594, 0.0006682824498373774944 ),
 .UNSPECIFIED. ) ;
#12262 = ORIENTED_EDGE ( 'NONE', *, *, #10954, .T. ) ;
#12263 = EDGE_LOOP ( 'NONE', ( #13652, #1111, #4844, #13613 ) ) ;
#12264 = CIRCLE ( 'NONE', #1664, 6.750000000000000000 ) ;
#12265 = CYLINDRICAL_SURFACE ( 'NONE', #2143, 4.199999999999981526 ) ;
#12266 = AXIS2_PLACEMENT_3D ( 'NONE', #6540, #9793, #14028 ) ;
#12267 = FACE_OUTER_BOUND ( 'NONE', #11142, .T. ) ;
#12268 = PRESENTATION_LAYER_ASSIGNMENT (  '', '', ( #12509 ) ) ;
#12269 = CARTESIAN_POINT ( 'NONE',  ( 0.000000000000000000, -3.464101615137757051, -1.999999999999996225 ) ) ;
#12270 = ORIENTED_EDGE ( 'NONE', *, *, #2718, .F. ) ;
#12271 = VECTOR ( 'NONE', #4358, 1000.000000000000000 ) ;
#12272 = EDGE_LOOP ( 'NONE', ( #8990, #10956, #12633, #2409 ) ) ;
#12273 = CARTESIAN_POINT ( 'NONE',  ( -10.00000000000000000, 371.6790804732683569, -190.0000000000000000 ) ) ;
#12274 = CARTESIAN_POINT ( 'NONE',  ( 635.0000000000000000, 160.0000000000000284, 207.0000000000000000 ) ) ;
#12275 = VECTOR ( 'NONE', #7023, 999.9999999999997726 ) ;
#12276 = DIRECTION ( 'NONE',  ( -0.000000000000000000, -1.000000000000000000, -0.000000000000000000 ) ) ;
#12277 = CARTESIAN_POINT ( 'NONE',  ( -6.259644161404860030E-16, -4.618802153517027165, -3.433295621305388234 ) ) ;
#12278 = SURFACE_STYLE_USAGE ( .BOTH. , #4464 ) ;
#12279 = SURFACE_STYLE_USAGE ( .BOTH. , #4394 ) ;
#12280 = EDGE_LOOP ( 'NONE', ( #3276, #14589, #14088, #4367 ) ) ;
#12281 = MECHANICAL_DESIGN_GEOMETRIC_PRESENTATION_REPRESENTATION (  '', ( #6640 ), #12057 ) ;
#12282 = DIRECTION ( 'NONE',  ( 0.000000000000000000, 0.000000000000000000, 1.000000000000000000 ) ) ;
#12283 = ORIENTED_EDGE ( 'NONE', *, *, #11221, .T. ) ;
#12284 = ORIENTED_EDGE ( 'NONE', *, *, #2118, .T. ) ;
#12285 = DIRECTION ( 'NONE',  ( 0.000000000000000000, 0.000000000000000000, -1.000000000000000000 ) ) ;
#12286 = ORIENTED_EDGE ( 'NONE', *, *, #13907, .T. ) ;
#12287 = VECTOR ( 'NONE', #6468, 1000.000000000000000 ) ;
#12288 = ADVANCED_FACE ( 'NONE', ( #9041 ), #3501, .F. ) ;
#12289 = ADVANCED_FACE ( 'NONE', ( #10288 ), #13689, .F. ) ;
#12290 = DIRECTION ( 'NONE',  ( 0.000000000000000000, 0.000000000000000000, 1.000000000000000000 ) ) ;
#12291 = MANIFOLD_SOLID_BREP ( 'EndChamfer', #9748 ) ;
#12292 = CARTESIAN_POINT ( 'NONE',  ( 0.000000000000000000, 0.000000000000000000, 4.000000000000000000 ) ) ;
#12293 = ORIENTED_EDGE ( 'NONE', *, *, #8891, .F. ) ;
#12294 = CARTESIAN_POINT ( 'NONE',  ( 6.271006797790669829, 0.9853839345309236553, 5.106080050406710313 ) ) ;
#12295 = DIRECTION ( 'NONE',  ( 0.000000000000000000, 0.000000000000000000, -1.000000000000000000 ) ) ;
#12296 = DIRECTION ( 'NONE',  ( -0.000000000000000000, -0.000000000000000000, -1.000000000000000000 ) ) ;
#12297 = DIRECTION ( 'NONE',  ( 0.000000000000000000, 0.000000000000000000, 1.000000000000000000 ) ) ;
#12298 = AXIS2_PLACEMENT_3D ( 'NONE', #1472, #6774, #2568 ) ;
#12299 = ORIENTED_EDGE ( 'NONE', *, *, #2218, .F. ) ;
#12300 = CARTESIAN_POINT ( 'NONE',  ( 6.371506350351446635, 5.409331239960136983, 0.8483282427581467777 ) ) ;
#12301 = VERTEX_POINT ( 'NONE', #12942 ) ;
#12302 = ORIENTED_EDGE ( 'NONE', *, *, #4776, .T. ) ;
#12303 = VERTEX_POINT ( 'NONE', #8363 ) ;
#12304 = DIRECTION ( 'NONE',  ( -0.5000000000000016653, 0.8660254037844378194, 0.000000000000000000 ) ) ;
#12305 = EDGE_CURVE ( 'NONE', #7148, #7687, #8560, .T. ) ;
#12306 = DIRECTION ( 'NONE',  ( -0.9578262852211513190, 0.2873478855663453846, 0.000000000000000000 ) ) ;
#12307 = AXIS2_PLACEMENT_3D ( 'NONE', #10599, #12742, #4928 ) ;
#12308 = CARTESIAN_POINT ( 'NONE',  ( 633.0483056743199768, 167.3094156464216269, -210.0000000000000284 ) ) ;
#12309 = AXIS2_PLACEMENT_3D ( 'NONE', #10876, #9981, #9700 ) ;
#12310 = LINE ( 'NONE', #2200, #3820 ) ;
#12311 = EDGE_CURVE ( 'NONE', #1544, #2949, #459, .T. ) ;
#12312 = EDGE_CURVE ( 'NONE', #6891, #9255, #12903, .T. ) ;
#12313 = DIRECTION ( 'NONE',  ( -1.000000000000000000, 0.000000000000000000, -0.000000000000000000 ) ) ;
#12314 = CARTESIAN_POINT ( 'NONE',  ( -9.018359789416532555E-15, -3.268109542640643905, 2.339468227445693937 ) ) ;
#12315 = LINE ( 'NONE', #3399, #12439 ) ;
#12316 = ORIENTED_EDGE ( 'NONE', *, *, #10596, .T. ) ;
#12317 = DIRECTION ( 'NONE',  ( 0.3420201433256622736, 0.000000000000000000, -0.9396926207859106484 ) ) ;
#12318 = CARTESIAN_POINT ( 'NONE',  ( 451.6722694765949768, 316.6998517015743460, -210.0000000000000000 ) ) ;
#12319 = PRODUCT_CONTEXT ( 'NONE', #6777, 'mechanical' ) ;
#12320 = CIRCLE ( 'NONE', #14224, 2.055000000000000160 ) ;
#12322 = AXIS2_PLACEMENT_3D ( 'NONE', #8206, #3877, #11672 ) ;
#12321 = CARTESIAN_POINT ( 'NONE',  ( 635.0000000000000000, 235.0000000000000284, -233.5000000000000000 ) ) ;
#12323 = EDGE_LOOP ( 'NONE', ( #3673, #7458, #8521, #6689 ) ) ;
#12324 = ORIENTED_EDGE ( 'NONE', *, *, #10084, .T. ) ;
#12325 = PRESENTATION_STYLE_ASSIGNMENT (( #14404 ) ) ;
#12326 = DIRECTION ( 'NONE',  ( 0.000000000000000000, 0.000000000000000000, 1.000000000000000000 ) ) ;
#12327 = EDGE_CURVE ( 'NONE', #3448, #5571, #11745, .T. ) ;
#12328 = CARTESIAN_POINT ( 'NONE',  ( -6.500000000000000000, 3.752776749732564809, -8.000000000000000000 ) ) ;
#12329 = B_SPLINE_CURVE_WITH_KNOTS ( 'NONE', 3,
 ( #5084, #9580, #13116, #7433, #8544, #3970 ),
 .UNSPECIFIED., .F., .F.,
 ( 4, 2, 4 ),
 ( -4.604908129294308270E-06, 0.0003318387708540395525, 0.0006682824498373734828 ),
 .UNSPECIFIED. ) ;
#12330 = CARTESIAN_POINT ( 'NONE',  ( 635.0000000000000000, 160.0000000000000284, 207.0000000000000000 ) ) ;
#12331 = ORIENTED_EDGE ( 'NONE', *, *, #10835, .F. ) ;
#12332 = EDGE_CURVE ( 'NONE', #214, #7052, #7257, .T. ) ;
#12333 = CARTESIAN_POINT ( 'NONE',  ( 630.0000000000000000, 160.0000000000000284, -222.5000000000000000 ) ) ;
#12334 = ORIENTED_EDGE ( 'NONE', *, *, #10660, .T. ) ;
#12335 = ADVANCED_FACE ( 'NONE', ( #11678 ), #11389, .F. ) ;
#12336 = DIRECTION ( 'NONE',  ( 0.000000000000000000, 0.000000000000000000, -1.000000000000000000 ) ) ;
#12337 = PRODUCT_DEFINITION ( 'UNKNOWN', '', #9252, #434 ) ;
#12338 = FACE_OUTER_BOUND ( 'NONE', #9711, .T. ) ;
#12339 = CARTESIAN_POINT ( 'NONE',  ( 0.000000000000000000, 0.000000000000000000, -8.000000000000000000 ) ) ;
#12340 = MANIFOLD_SOLID_BREP ( 'EndChamfer', #6212 ) ;
#12341 = ORIENTED_EDGE ( 'NONE', *, *, #106, .F. ) ;
#12342 = ORIENTED_EDGE ( 'NONE', *, *, #13536, .T. ) ;
#12343 = CARTESIAN_POINT ( 'NONE',  ( 4.207491450040567571, -2.029819825146485179, -3.671670828759567407 ) ) ;
#12344 = APPLICATION_CONTEXT ( 'automotive_design' ) ;
#12345 = DIRECTION ( 'NONE',  ( 0.000000000000000000, 0.4999999999999990563, -0.8660254037844391517 ) ) ;
#12346 = DIRECTION ( 'NONE',  ( 0.000000000000000000, 0.000000000000000000, -1.000000000000000000 ) ) ;
#12347 = ORIENTED_EDGE ( 'NONE', *, *, #561, .T. ) ;
#12348 = LINE ( 'NONE', #13604, #8089 ) ;
#12349 = CARTESIAN_POINT ( 'NONE',  ( 2.141486166123590884, -6.269165884987830673, -0.07763482564821427845 ) ) ;
#12350 = DIRECTION ( 'NONE',  ( 1.000000000000000000, 0.000000000000000000, 0.000000000000000000 ) ) ;
#12351 = CARTESIAN_POINT ( 'NONE',  ( 629.0000000000000000, 154.0000000000000284, 187.5000000000000000 ) ) ;
#12352 = CARTESIAN_POINT ( 'NONE',  ( 0.6666666666666658525, -4.233901974057276085, -3.300726591567086476 ) ) ;
#12353 =( NAMED_UNIT ( * ) PLANE_ANGLE_UNIT ( ) SI_UNIT ( $, .RADIAN. ) );
#12354 = ORIENTED_EDGE ( 'NONE', *, *, #617, .T. ) ;
#12355 = CARTESIAN_POINT ( 'NONE',  ( 148.9991633467111569, 386.6211705227183870, 210.0000000000000000 ) ) ;
#12356 = VERTEX_POINT ( 'NONE', #2751 ) ;
#12357 = ORIENTED_EDGE ( 'NONE', *, *, #5278, .F. ) ;
#12358 = LINE ( 'NONE', #13615, #8040 ) ;
#12359 = EDGE_CURVE ( 'NONE', #1880, #6883, #11529, .T. ) ;
#12360 = ORIENTED_EDGE ( 'NONE', *, *, #11454, .T. ) ;
#12361 = EDGE_CURVE ( 'NONE', #10329, #4518, #9154, .T. ) ;
#12362 = DIRECTION ( 'NONE',  ( -0.000000000000000000, -0.000000000000000000, 1.000000000000000000 ) ) ;
#12363 = DIRECTION ( 'NONE',  ( 0.000000000000000000, 0.000000000000000000, 1.000000000000000000 ) ) ;
#12364 = ORIENTED_EDGE ( 'NONE', *, *, #6995, .F. ) ;
#12365 = DIRECTION ( 'NONE',  ( 9.794481010665704304E-16, 3.264827003555234768E-15, -1.000000000000000000 ) ) ;
#12366 = CARTESIAN_POINT ( 'NONE',  ( 636.9746078850427011, 155.6249658629529620, -210.0000000000000000 ) ) ;
#12367 = CARTESIAN_POINT ( 'NONE',  ( -1.604619215278546562E-14, -7.505553499465138501, -0.8000000000000003775 ) ) ;
#12368 = DIRECTION ( 'NONE',  ( -0.8660254037844373753, 0.5000000000000021094, 0.000000000000000000 ) ) ;
#12369 = SURFACE_SIDE_STYLE ('',( #2327 ) ) ;
#12370 = ORIENTED_EDGE ( 'NONE', *, *, #12485, .F. ) ;
#12372 = EDGE_CURVE ( 'NONE', #6378, #3582, #3725, .T. ) ;
#12371 = DIRECTION ( 'NONE',  ( -0.000000000000000000, 1.000000000000000000, -0.000000000000000000 ) ) ;
#12373 = VERTEX_POINT ( 'NONE', #9332 ) ;
#12374 = AXIS2_PLACEMENT_3D ( 'NONE', #1707, #3922, #7168 ) ;
#12375 = ORIENTED_EDGE ( 'NONE', *, *, #5239, .F. ) ;
#12376 = DIRECTION ( 'NONE',  ( 0.000000000000000000, 0.000000000000000000, -1.000000000000000000 ) ) ;
#12377 = LINE ( 'NONE', #14464, #6132 ) ;
#12378 = CARTESIAN_POINT ( 'NONE',  ( 707.0389973793284071, 162.8315651648150606, -177.6000000000005059 ) ) ;
#12379 = FACE_BOUND ( 'NONE', #9665, .T. ) ;
#12380 = LINE ( 'NONE', #11279, #983 ) ;
#12381 = LINE ( 'NONE', #108, #5665 ) ;
#12382 = CARTESIAN_POINT ( 'NONE',  ( 0.000000000000000000, 0.000000000000000000, -0.4621369752184044666 ) ) ;
#12383 = ADVANCED_FACE ( 'NONE', ( #13830 ), #2620, .F. ) ;
#12384 = ORIENTED_EDGE ( 'NONE', *, *, #2770, .T. ) ;
#12385 = CARTESIAN_POINT ( 'NONE',  ( -5.727634848076946561, -4.575561887448768239, -6.326622577870699260 ) ) ;
#12386 = LINE ( 'NONE', #8928, #2088 ) ;
#12387 = APPLICATION_PROTOCOL_DEFINITION ( 'draft international standard', 'automotive_design', 1998, #8854 ) ;
#12388 = CARTESIAN_POINT ( 'NONE',  ( -8.505790995054899994, 376.6597771564184427, -184.8000000000000398 ) ) ;
#12389 = ORIENTED_EDGE ( 'NONE', *, *, #2288, .F. ) ;
#12390 = ORIENTED_EDGE ( 'NONE', *, *, #7410, .T. ) ;
#12391 = DIRECTION ( 'NONE',  ( 0.000000000000000000, 0.000000000000000000, 1.000000000000000000 ) ) ;
#12392 = FACE_OUTER_BOUND ( 'NONE', #11443, .T. ) ;
#12393 = PRODUCT ( 'hex bolt gradeab_iso_ISO 4014 - M5 x 30 x 16-N', 'hex bolt gradeab_iso_ISO 4014 - M5 x 30 x 16-N', '', ( #9757 ) ) ;
#12394 = CARTESIAN_POINT ( 'NONE',  ( -4.000000000000000000, -2.309401076758512694, -3.433295621305382461 ) ) ;
#12395 = PLANE ( 'NONE',  #11013 ) ;
#12396 = ADVANCED_FACE ( 'NONE', ( #4910 ), #5123, .T. ) ;
#12397 = VERTEX_POINT ( 'NONE', #9775 ) ;
#12398 = DIRECTION ( 'NONE',  ( -1.000000000000000000, -0.000000000000000000, -0.000000000000000000 ) ) ;
#12399 = LINE ( 'NONE', #6879, #3744 ) ;
#12400 =( LENGTH_UNIT ( ) NAMED_UNIT ( * ) SI_UNIT ( .MILLI., .METRE. ) );
#12401 = ADVANCED_FACE ( 'NONE', ( #8736 ), #7635, .F. ) ;
#12402 = CARTESIAN_POINT ( 'NONE',  ( 451.6722694765949768, 316.6998517015743460, -190.0000000000000000 ) ) ;
#12403 = VERTEX_POINT ( 'NONE', #8514 ) ;
#12404 = ORIENTED_EDGE ( 'NONE', *, *, #11278, .F. ) ;
#12405 = CARTESIAN_POINT ( 'NONE',  ( 4.197393957002303999, 7.772902908466098641E-14, -3.503767560748929810 ) ) ;
#12406 = EDGE_CURVE ( 'NONE', #5548, #11364, #8589, .T. ) ;
#12407 = CARTESIAN_POINT ( 'NONE',  ( 635.0000000000000000, 160.0000000000000284, -222.5000000000000000 ) ) ;
#12408 = EDGE_CURVE ( 'NONE', #7500, #4931, #10336, .T. ) ;
#12409 = CARTESIAN_POINT ( 'NONE',  ( -20.63749999999999574, 0.000000000000000000, 0.000000000000000000 ) ) ;
#12410 = EDGE_CURVE ( 'NONE', #5305, #3847, #6520, .T. ) ;
#12411 = B_SPLINE_CURVE_WITH_KNOTS ( 'NONE', 3,
 ( #6330, #13488, #13622, #1230, #7807, #14519 ),
 .UNSPECIFIED., .F., .F.,
 ( 4, 2, 4 ),
 ( 0.008261945092156346496, 0.009724140865920691962, 0.01118633663968503569 ),
 .UNSPECIFIED. ) ;
#12413 = ORIENTED_EDGE ( 'NONE', *, *, #14317, .F. ) ;
#12412 = AXIS2_PLACEMENT_3D ( 'NONE', #11143, #12236, #8636 ) ;
#12414 = VECTOR ( 'NONE', #5072, 1000.000000000000000 ) ;
#12415 = ORIENTED_EDGE ( 'NONE', *, *, #9713, .T. ) ;
#12416 = DIRECTION ( 'NONE',  ( 1.000000000000000000, 0.000000000000000000, 0.000000000000000000 ) ) ;
#12417 = CARTESIAN_POINT ( 'NONE',  ( 635.0000000000000000, 160.0000000000000284, 211.0000000000000000 ) ) ;
#12418 = CARTESIAN_POINT ( 'NONE',  ( -10.00000000000000888, 371.6790804732683569, -169.9999999999999716 ) ) ;
#12419 = CARTESIAN_POINT ( 'NONE',  ( 650.0000000000000000, 145.0000000000000568, 210.0000000000000000 ) ) ;
#12420 = EDGE_LOOP ( 'NONE', ( #12808, #3436, #13716, #8749 ) ) ;
#12421 = CYLINDRICAL_SURFACE ( 'NONE', #9434, 4.199999999999981526 ) ;
#12422 = ORIENTED_EDGE ( 'NONE', *, *, #9942, .F. ) ;
#12423 = ORIENTED_EDGE ( 'NONE', *, *, #2742, .T. ) ;
#12424 = DIRECTION ( 'NONE',  ( 0.000000000000000000, 0.8660254037844375974, -0.5000000000000018874 ) ) ;
#12425 = EDGE_CURVE ( 'NONE', #4571, #13301, #10947, .T. ) ;
#12426 = ADVANCED_FACE ( 'NONE', ( #6293 ), #674, .T. ) ;
#12427 = ORIENTED_EDGE ( 'NONE', *, *, #4847, .F. ) ;
#12428 = AXIS2_PLACEMENT_3D ( 'NONE', #12419, #6896, #5507 ) ;
#12429 = ADVANCED_FACE ( 'NONE', ( #13304 ), #13239, .F. ) ;
#12430 = DIRECTION ( 'NONE',  ( 0.000000000000000000, 0.000000000000000000, 1.000000000000000000 ) ) ;
#12431 = FACE_OUTER_BOUND ( 'NONE', #6833, .T. ) ;
#12432 = ORIENTED_EDGE ( 'NONE', *, *, #5808, .F. ) ;
#12433 = DIRECTION ( 'NONE',  ( 0.000000000000000000, 0.000000000000000000, -1.000000000000000000 ) ) ;
#12434 = PLANE ( 'NONE',  #12231 ) ;
#12435 = CIRCLE ( 'NONE', #3022, 0.5155456020628804703 ) ;
#12436 = AXIS2_PLACEMENT_3D ( 'NONE', #7554, #11087, #888 ) ;
#12437 = LINE ( 'NONE', #2325, #7007 ) ;
#12438 = FACE_OUTER_BOUND ( 'NONE', #13293, .T. ) ;
#12439 = VECTOR ( 'NONE', #11362, 1000.000000000000000 ) ;
#12440 = ORIENTED_EDGE ( 'NONE', *, *, #13505, .F. ) ;
#12441 = LINE ( 'NONE', #7885, #2582 ) ;
#12442 = ORIENTED_EDGE ( 'NONE', *, *, #4089, .T. ) ;
#12443 = EDGE_LOOP ( 'NONE', ( #4675, #8959, #2661, #10067 ) ) ;
#12444 = CARTESIAN_POINT ( 'NONE',  ( 4.574783636564889733, -5.228990388888015595, -6.171384342982775273 ) ) ;
#12445 = VECTOR ( 'NONE', #10547, 1000.000000000000000 ) ;
#12446 = CARTESIAN_POINT ( 'NONE',  ( -20.63749999999999929, 0.000000000000000000, -5.525000000000000355 ) ) ;
#12447 = DIRECTION ( 'NONE',  ( 0.000000000000000000, 0.000000000000000000, -1.000000000000000000 ) ) ;
#12448 = CARTESIAN_POINT ( 'NONE',  ( -3.309651814758565180, -5.455921364805393026, -1.000000000000000000 ) ) ;
#12449 = CARTESIAN_POINT ( 'NONE',  ( 6.367873360227559232, -5.773502691896264416, 0.000000000000000000 ) ) ;
#12450 = DIRECTION ( 'NONE',  ( 1.000000000000000000, 0.000000000000000000, 0.000000000000000000 ) ) ;
#12451 = DIRECTION ( 'NONE',  ( 1.000000000000000000, 0.000000000000000000, 0.000000000000000000 ) ) ;
#12452 = ORIENTED_EDGE ( 'NONE', *, *, #3786, .T. ) ;
#12453 = VECTOR ( 'NONE', #4540, 1000.000000000000227 ) ;
#12454 = VECTOR ( 'NONE', #10108, 1000.000000000000000 ) ;
#12455 = DIRECTION ( 'NONE',  ( 0.2873478855663453846, 0.9578262852211513190, 0.000000000000000000 ) ) ;
#12456 = CARTESIAN_POINT ( 'NONE',  ( -6.725979247667767780, -3.622307570260316911, -6.470294263593358686 ) ) ;
#12457 = DIRECTION ( 'NONE',  ( 0.000000000000000000, 0.000000000000000000, -1.000000000000000000 ) ) ;
#12458 = SHAPE_DEFINITION_REPRESENTATION ( #3343, #3392 ) ;
#12459 = EDGE_LOOP ( 'NONE', ( #7380, #6231, #7339, #7537, #12679 ) ) ;
#12460 = PLANE ( 'NONE',  #3314 ) ;
#12461 = VERTEX_POINT ( 'NONE', #13024 ) ;
#12462 = ORIENTED_EDGE ( 'NONE', *, *, #2670, .T. ) ;
#12463 = FILL_AREA_STYLE_COLOUR ( '', #3257 ) ;
#12464 = FACE_OUTER_BOUND ( 'NONE', #8277, .T. ) ;
#12465 = AXIS2_PLACEMENT_3D ( 'NONE', #5374, #4131, #7512 ) ;
#12466 = CARTESIAN_POINT ( 'NONE',  ( 2.500000000000000000, 2.357898499370431722, -2.818925648462311528E-15 ) ) ;
#12467 = EDGE_CURVE ( 'NONE', #13064, #14191, #11008, .T. ) ;
#12468 = AXIS2_PLACEMENT_3D ( 'NONE', #4138, #1915, #12015 ) ;
#12469 = AXIS2_PLACEMENT_3D ( 'NONE', #14300, #6486, #12150 ) ;
#12470 = DIRECTION ( 'NONE',  ( 0.000000000000000000, 0.000000000000000000, -1.000000000000000000 ) ) ;
#12471 = DIRECTION ( 'NONE',  ( 0.000000000000000000, 0.000000000000000000, -1.000000000000000000 ) ) ;
#12472 = ORIENTED_EDGE ( 'NONE', *, *, #4100, .T. ) ;
#12473 =( GEOMETRIC_REPRESENTATION_CONTEXT ( 3 ) GLOBAL_UNCERTAINTY_ASSIGNED_CONTEXT ( ( #9156 ) ) GLOBAL_UNIT_ASSIGNED_CONTEXT ( ( #8453, #618, #13110 ) ) REPRESENTATION_CONTEXT ( 'NONE', 'WORKASPACE' ) );
#12474 = DIRECTION ( 'NONE',  ( 0.9578262852211525402, -0.2873478855663419429, -0.000000000000000000 ) ) ;
#12475 = CARTESIAN_POINT ( 'NONE',  ( 590.0000000000000000, 10.00000000000005507, -210.0020000000000095 ) ) ;
#12476 = VECTOR ( 'NONE', #8835, 1000.000000000000000 ) ;
#12477 = CARTESIAN_POINT ( 'NONE',  ( 636.7009106935324780, 155.5114698605638637, -211.0000000000000000 ) ) ;
#12478 = VECTOR ( 'NONE', #4250, 1000.000000000000000 ) ;
#12479 = VERTEX_POINT ( 'NONE', #7413 ) ;
#12480 = VERTEX_POINT ( 'NONE', #11898 ) ;
#12481 = CARTESIAN_POINT ( 'NONE',  ( 6.837824896291514243, -3.947820044545437224, -6.564402953523717166 ) ) ;
#12482 = DIRECTION ( 'NONE',  ( -0.9578262852211514300, 0.2873478855663454401, 0.000000000000000000 ) ) ;
#12483 = CARTESIAN_POINT ( 'NONE',  ( 610.0000000000001137, 185.6790804732683853, -169.9999999999999716 ) ) ;
#12484 = AXIS2_PLACEMENT_3D ( 'NONE', #6790, #5542, #3338 ) ;
#12485 = EDGE_CURVE ( 'NONE', #6858, #7340, #9706, .T. ) ;
#12486 = VECTOR ( 'NONE', #14491, 1000.000000000000000 ) ;
#12487 = CARTESIAN_POINT ( 'NONE',  ( 6.212068001623188174, 5.350125758160983125, -0.7333103599822197172 ) ) ;
#12488 = ADVANCED_FACE ( 'NONE', ( #5197 ), #14206, .T. ) ;
#12489 = AXIS2_PLACEMENT_3D ( 'NONE', #13702, #3600, #2318 ) ;
#12490 = ORIENTED_EDGE ( 'NONE', *, *, #9956, .T. ) ;
#12491 = VECTOR ( 'NONE', #9294, 1000.000000000000114 ) ;
#12492 = CARTESIAN_POINT ( 'NONE',  ( -1.500000000000001332, 0.000000000000000000, 0.000000000000000000 ) ) ;
#12493 = CARTESIAN_POINT ( 'NONE',  ( 610.0000000000001137, 185.6790804732684990, -184.8000000000000966 ) ) ;
#12494 = DIRECTION ( 'NONE',  ( -0.000000000000000000, -0.000000000000000000, -1.000000000000000000 ) ) ;
#12495 = EDGE_CURVE ( 'NONE', #7242, #3214, #7476, .T. ) ;
#12496 = LINE ( 'NONE', #6895, #13859 ) ;
#12497 = FACE_OUTER_BOUND ( 'NONE', #2815, .T. ) ;
#12498 = CARTESIAN_POINT ( 'NONE',  ( -9.137956343300853490, 374.5525593289319204, 184.8000000000000398 ) ) ;
#12499 = CARTESIAN_POINT ( 'NONE',  ( 0.000000000000000000, 0.000000000000000000, 0.000000000000000000 ) ) ;
#12500 = CIRCLE ( 'NONE', #9694, 2.649999999999985700 ) ;
#12501 = ORIENTED_EDGE ( 'NONE', *, *, #10772, .F. ) ;
#12502 = VECTOR ( 'NONE', #8795, 1000.000000000000000 ) ;
#12503 = EDGE_CURVE ( 'NONE', #8880, #6036, #11968, .T. ) ;
#12504 = DIRECTION ( 'NONE',  ( -0.9578262852211506528, 0.2873478855663477161, -0.000000000000000000 ) ) ;
#12505 = EDGE_LOOP ( 'NONE', ( #5730, #14523 ) ) ;
#12506 = ORIENTED_EDGE ( 'NONE', *, *, #10703, .T. ) ;
#12507 = LINE ( 'NONE', #3509, #1911 ) ;
#12508 = VECTOR ( 'NONE', #8100, 1000.000000000000114 ) ;
#12509 = STYLED_ITEM ( 'NONE', ( #10302 ), #6538 ) ;
#12510 = VERTEX_POINT ( 'NONE', #6376 ) ;
#12511 = CARTESIAN_POINT ( 'NONE',  ( -9.498873539028489220E-16, 10.00000000000000000, -210.0000000000000000 ) ) ;
#12512 = AXIS2_PLACEMENT_3D ( 'NONE', #3619, #4577, #12607 ) ;
#12513 = VECTOR ( 'NONE', #1733, 1000.000000000000000 ) ;
#12514 = DIRECTION ( 'NONE',  ( 0.8191520442889917986, 1.003171929053524747E-16, -0.5735764363510460484 ) ) ;
#12515 = ORIENTED_EDGE ( 'NONE', *, *, #4126, .T. ) ;
#12516 = CARTESIAN_POINT ( 'NONE',  ( 8.500000000000000000, 0.000000000000000000, 4.000000000000000000 ) ) ;
#12517 = DIRECTION ( 'NONE',  ( 0.000000000000000000, -1.000000000000000000, 0.000000000000000000 ) ) ;
#12518 = AXIS2_PLACEMENT_3D ( 'NONE', #7726, #5445, #9947 ) ;
#12519 = EDGE_CURVE ( 'NONE', #8892, #4166, #14341, .T. ) ;
#12520 = ADVANCED_BREP_SHAPE_REPRESENTATION ( '', ( #11971, #9440 ), #8508 ) ;
#12521 = DIRECTION ( 'NONE',  ( 0.2873478855663483267, 0.9578262852211504308, 0.000000000000000000 ) ) ;
#12522 = DIRECTION ( 'NONE',  ( -1.000000000000000000, 0.000000000000000000, 0.000000000000000000 ) ) ;
#12523 = VERTEX_POINT ( 'NONE', #757 ) ;
#12524 = EDGE_CURVE ( 'NONE', #12114, #11816, #5388, .T. ) ;
#12525 = FACE_OUTER_BOUND ( 'NONE', #7141, .T. ) ;
#12526 = PRODUCT_RELATED_PRODUCT_CATEGORY ( 'part', '', ( #12393 ) ) ;
#12527 = VERTEX_POINT ( 'NONE', #2004 ) ;
#12528 = CIRCLE ( 'NONE', #9483, 4.000000000000000000 ) ;
#12529 = ORIENTED_EDGE ( 'NONE', *, *, #6463, .F. ) ;
#12530 = CARTESIAN_POINT ( 'NONE',  ( 5.589124336234546853, -4.278671059401403021, -6.219623095963592974 ) ) ;
#12531 = PRODUCT ( 'socket head cap screw_iso_ISO 4762 M5 x 16 - 16N', 'socket head cap screw_iso_ISO 4762 M5 x 16 - 16N', '', ( #10109 ) ) ;
#12532 = COLOUR_RGB ( '',1.000000000000000000, 0.9490196078431372140, 0.9098039215686274384 ) ;
#12533 = CARTESIAN_POINT ( 'NONE',  ( 610.0000000000002274, 191.1080398579018720, -187.0000000000000284 ) ) ;
#12534 = CARTESIAN_POINT ( 'NONE',  ( 726.1975094929946408, 167.5243180396263938, 150.0000000000013642 ) ) ;
#12535 = AXIS2_PLACEMENT_3D ( 'NONE', #10080, #6977, #10233 ) ;
#12536 = DIRECTION ( 'NONE',  ( 1.000000000000000000, 0.000000000000000000, 0.000000000000000000 ) ) ;
#12537 = DIRECTION ( 'NONE',  ( 0.000000000000000000, 0.000000000000000000, -1.000000000000000000 ) ) ;
#12538 = DIRECTION ( 'NONE',  ( -3.469446951953611033E-15, -1.000000000000000000, 0.000000000000000000 ) ) ;
#12539 = LINE ( 'NONE', #10319, #194 ) ;
#12540 = ORIENTED_EDGE ( 'NONE', *, *, #7246, .F. ) ;
#12541 = AXIS2_PLACEMENT_3D ( 'NONE', #9162, #10489, #9469 ) ;
#12542 = CARTESIAN_POINT ( 'NONE',  ( 0.000000000000000000, 0.000000000000000000, -5.000000000000000000 ) ) ;
#12543 = CARTESIAN_POINT ( 'NONE',  ( 0.000000000000000000, 0.000000000000000000, 0.000000000000000000 ) ) ;
#12544 = DIRECTION ( 'NONE',  ( -0.000000000000000000, -0.000000000000000000, 1.000000000000000000 ) ) ;
#12545 = CONTEXT_DEPENDENT_SHAPE_REPRESENTATION ( #11121, #10768 ) ;
#12546 = ORIENTED_EDGE ( 'NONE', *, *, #2889, .F. ) ;
#12547 = CARTESIAN_POINT ( 'NONE',  ( 628.0000000000000000, 242.0000000000000568, -225.5000000000000000 ) ) ;
#12548 = EDGE_LOOP ( 'NONE', ( #6461, #7612, #14130, #13391 ) ) ;
#12549 = ORIENTED_EDGE ( 'NONE', *, *, #13630, .T. ) ;
#12550 = VECTOR ( 'NONE', #5370, 1000.000000000000000 ) ;
#12551 = FILL_AREA_STYLE ('',( #12463 ) ) ;
#12552 = CARTESIAN_POINT ( 'NONE',  ( 6.367873360227556567, 2.886751345948122882, -5.000000000000000000 ) ) ;
#12553 = EDGE_CURVE ( 'NONE', #5458, #2876, #14421, .T. ) ;
#12554 = LINE ( 'NONE', #11507, #14137 ) ;
#12555 = EDGE_CURVE ( 'NONE', #3640, #5396, #11163, .T. ) ;
#12556 = DIRECTION ( 'NONE',  ( -1.000000000000000000, -0.000000000000000000, -0.000000000000000000 ) ) ;
#12557 = UNCERTAINTY_MEASURE_WITH_UNIT (LENGTH_MEASURE( 1.000000000000000082E-05 ), #8212, 'distance_accuracy_value', 'NONE');
#12558 = AXIS2_PLACEMENT_3D ( 'NONE', #9870, #5521, #2107 ) ;
#12559 = DIRECTION ( 'NONE',  ( -0.9578262852211517631, 0.2873478855663438858, -0.000000000000000000 ) ) ;
#12560 = ORIENTED_EDGE ( 'NONE', *, *, #9811, .T. ) ;
#12561 = VECTOR ( 'NONE', #9617, 1000.000000000000000 ) ;
#12562 = DIRECTION ( 'NONE',  ( -0.2873478855663446629, -0.9578262852211516520, 0.000000000000000000 ) ) ;
#12563 = CARTESIAN_POINT ( 'NONE',  ( 708.1388811837592812, 164.7984674554473372, 182.8000000000001535 ) ) ;
#12564 = CARTESIAN_POINT ( 'NONE',  ( 139.8040310085880833, 355.9707293956415697, 183.5000000000000000 ) ) ;
#12565 = PRODUCT_DEFINITION_SHAPE ( 'NONE', 'NONE',  #14642 ) ;
#12566 = CARTESIAN_POINT ( 'NONE',  ( 639.0000000000000000, 156.0000000000000000, -233.5000000000000000 ) ) ;
#12567 = ADVANCED_FACE ( 'NONE', ( #5771 ), #13454, .T. ) ;
#12568 = ORIENTED_EDGE ( 'NONE', *, *, #12054, .T. ) ;
#12569 = VERTEX_POINT ( 'NONE', #9092 ) ;
#12570 = DIRECTION ( 'NONE',  ( -0.000000000000000000, -0.000000000000000000, -1.000000000000000000 ) ) ;
#12571 = LINE ( 'NONE', #10651, #188 ) ;
#12572 = CARTESIAN_POINT ( 'NONE',  ( 4.204115023516791005, -1.660442669500199919, -3.602151381774560068 ) ) ;
#12573 = ORIENTED_EDGE ( 'NONE', *, *, #1499, .T. ) ;
#12574 = ORIENTED_EDGE ( 'NONE', *, *, #1404, .F. ) ;
#12575 = FACE_OUTER_BOUND ( 'NONE', #8131, .T. ) ;
#12576 = LINE ( 'NONE', #7254, #3067 ) ;
#12577 = CARTESIAN_POINT ( 'NONE',  ( 640.2500000000000000, 160.0000000000000284, 207.0000000000000000 ) ) ;
#12578 = DIRECTION ( 'NONE',  ( 3.072361293536515954E-16, -4.159212477520619976E-15, -1.000000000000000000 ) ) ;
#12579 = FILL_AREA_STYLE_COLOUR ( '', #6448 ) ;
#12580 =( LENGTH_UNIT ( ) NAMED_UNIT ( * ) SI_UNIT ( .MILLI., .METRE. ) );
#12581 = EDGE_CURVE ( 'NONE', #9710, #11130, #8447, .T. ) ;
#12582 = ORIENTED_EDGE ( 'NONE', *, *, #6012, .F. ) ;
#12583 = CARTESIAN_POINT ( 'NONE',  ( 641.0000000000000000, 166.0000000000000284, 187.5000000000000000 ) ) ;
#12584 = ORIENTED_EDGE ( 'NONE', *, *, #9413, .T. ) ;
#12585 = EDGE_LOOP ( 'NONE', ( #11327, #13784, #7003, #7428 ) ) ;
#12586 = CARTESIAN_POINT ( 'NONE',  ( 0.000000000000000000, 0.000000000000000000, 0.000000000000000000 ) ) ;
#12587 = FACE_OUTER_BOUND ( 'NONE', #8048, .T. ) ;
#12588 = LINE ( 'NONE', #12734, #4052 ) ;
#12589 = ORIENTED_EDGE ( 'NONE', *, *, #9352, .T. ) ;
#12590 = PLANE ( 'NONE',  #6185 ) ;
#12591 = CARTESIAN_POINT ( 'NONE',  ( -8.331345277524542681, 1.033251829022860324E-15, -8.000000000000000000 ) ) ;
#12592 = LINE ( 'NONE', #2476, #11935 ) ;
#12593 = DIRECTION ( 'NONE',  ( 0.000000000000000000, 0.000000000000000000, -1.000000000000000000 ) ) ;
#12594 = ADVANCED_FACE ( 'NONE', ( #3349 ), #10123, .F. ) ;
#12595 = ORIENTED_EDGE ( 'NONE', *, *, #3834, .F. ) ;
#12596 = CARTESIAN_POINT ( 'NONE',  ( 631.0000000000000000, 164.0000000000000284, -233.5000000000000000 ) ) ;
#12597 = AXIS2_PLACEMENT_3D ( 'NONE', #13428, #6857, #12451 ) ;
#12598 = VERTEX_POINT ( 'NONE', #12563 ) ;
#12599 = ORIENTED_EDGE ( 'NONE', *, *, #498, .T. ) ;
#12600 = FACE_OUTER_BOUND ( 'NONE', #1431, .T. ) ;
#12601 = EDGE_CURVE ( 'NONE', #13081, #2565, #3984, .T. ) ;
#12602 = EDGE_CURVE ( 'NONE', #5031, #12986, #12208, .T. ) ;
#12603 = CARTESIAN_POINT ( 'NONE',  ( 639.0000000000000000, 156.0000000000000000, -233.5000000000000000 ) ) ;
#12604 = CARTESIAN_POINT ( 'NONE',  ( 0.000000000000000000, -4.330127018922189208, 2.500000000000010658 ) ) ;
#12605 = EDGE_CURVE ( 'NONE', #2635, #7765, #10272, .T. ) ;
#12606 = EDGE_LOOP ( 'NONE', ( #3418, #3884, #11892, #10226, #7259, #11211 ) ) ;
#12607 = DIRECTION ( 'NONE',  ( 0.000000000000000000, 1.000000000000000000, 0.000000000000000000 ) ) ;
#12608 = DIRECTION ( 'NONE',  ( 0.000000000000000000, -1.000000000000000000, 0.000000000000000000 ) ) ;
#12609 = CARTESIAN_POINT ( 'NONE',  ( -0.1481481481481481122, -4.797713218419819903, 0.000000000000000000 ) ) ;
#12610 = DIRECTION ( 'NONE',  ( 9.463134714538378657E-16, -7.093113185993356941E-16, -1.000000000000000000 ) ) ;
#12611 = EDGE_LOOP ( 'NONE', ( #8195, #1827, #8313 ) ) ;
#12612 = CARTESIAN_POINT ( 'NONE',  ( 6.534838248920899595, -2.951765777552421532, -5.112608298763837489 ) ) ;
#12613 = CARTESIAN_POINT ( 'NONE',  ( 0.04050535873993867109, -7.919512791578240396, -6.573129608219095310 ) ) ;
#12614 = CARTESIAN_POINT ( 'NONE',  ( 610.2366331756301179, 189.6374102278066971, 186.5502271136477361 ) ) ;
#12615 = ORIENTED_EDGE ( 'NONE', *, *, #8848, .F. ) ;
#12616 = LINE ( 'NONE', #419, #3574 ) ;
#12617 = ORIENTED_EDGE ( 'NONE', *, *, #12425, .T. ) ;
#12618 = EDGE_LOOP ( 'NONE', ( #5561, #5540, #13123, #414 ) ) ;
#12619 = CARTESIAN_POINT ( 'NONE',  ( 610.0000000000000000, -9.999999999999941380, -210.0000000000000000 ) ) ;
#12620 = CARTESIAN_POINT ( 'NONE',  ( 0.04050535873994059316, 7.919512791578233291, -6.573129608219092646 ) ) ;
#12621 = EDGE_CURVE ( 'NONE', #7939, #8737, #11228, .T. ) ;
#12622 = CARTESIAN_POINT ( 'NONE',  ( -6.837824896291515131, -3.947820044545435447, -6.564402953523717166 ) ) ;
#12623 =( REPRESENTATION_RELATIONSHIP ('NONE','NONE', #2822, #14430 ) REPRESENTATION_RELATIONSHIP_WITH_TRANSFORMATION ( #13432 )SHAPE_REPRESENTATION_RELATIONSHIP( ) );
#12624 = CARTESIAN_POINT ( 'NONE',  ( 5.699988423468465015, 4.591578518468247161, -6.344710093416081165 ) ) ;
#12625 = CARTESIAN_POINT ( 'NONE',  ( 9.498873539028489220E-16, -10.00000000000000000, 210.0000000000000000 ) ) ;
#12626 = ORIENTED_EDGE ( 'NONE', *, *, #5594, .F. ) ;
#12627 = EDGE_CURVE ( 'NONE', #12082, #12943, #11089, .T. ) ;
#12628 = CARTESIAN_POINT ( 'NONE',  ( 2.500000000000000000, 1.178949249685217415, 2.041999999999998483 ) ) ;
#12629 = CARTESIAN_POINT ( 'NONE',  ( 139.8040310085880833, 355.9707293956415697, -190.0000000000000000 ) ) ;
#12630 = DIRECTION ( 'NONE',  ( 1.000000000000000000, 0.000000000000000000, 0.000000000000000000 ) ) ;
#12631 = EDGE_CURVE ( 'NONE', #3596, #11200, #12399, .T. ) ;
#12632 = DIRECTION ( 'NONE',  ( 1.000000000000000000, 0.000000000000000000, 0.000000000000000000 ) ) ;
#12633 = ORIENTED_EDGE ( 'NONE', *, *, #3856, .T. ) ;
#12634 = EDGE_LOOP ( 'NONE', ( #5066, #11187, #932, #7750, #5752, #842, #292, #6753, #11753, #586, #6971, #7221, #5572, #5886, #13894, #2241, #11715, #5270, #2882, #7796 ) ) ;
#12635 = CARTESIAN_POINT ( 'NONE',  ( 631.2228576472183477, 153.4466020873430239, 210.0000120000000265 ) ) ;
#12636 = DIRECTION ( 'NONE',  ( -0.000000000000000000, -0.000000000000000000, 1.000000000000000000 ) ) ;
#12637 = CARTESIAN_POINT ( 'NONE',  ( 6.212068001622437663, 3.310128279683251851, 4.266689640018040741 ) ) ;
#12638 = ORIENTED_EDGE ( 'NONE', *, *, #9050, .F. ) ;
#12639 = ORIENTED_EDGE ( 'NONE', *, *, #3315, .T. ) ;
#12640 = CARTESIAN_POINT ( 'NONE',  ( 10.00000000000000000, 10.00000000000000178, -210.0020000000000095 ) ) ;
#12641 = DIRECTION ( 'NONE',  ( -1.000000000000000000, -0.000000000000000000, -0.000000000000000000 ) ) ;
#12642 = CARTESIAN_POINT ( 'NONE',  ( 6.527192678185238961, 5.883244248022512224, -1.510895765055974796E-13 ) ) ;
#12643 = CARTESIAN_POINT ( 'NONE',  ( 3.999999999999999112, 4.898587196589411843E-16, -7.974599999999998801 ) ) ;
#12644 = CARTESIAN_POINT ( 'NONE',  ( -1.126429428730189031, 7.232124035235028892, -6.344710093416086494 ) ) ;
#12645 =( LENGTH_UNIT ( ) NAMED_UNIT ( * ) SI_UNIT ( .MILLI., .METRE. ) );
#12646 = EDGE_LOOP ( 'NONE', ( #4621, #1104 ) ) ;
#12647 = CARTESIAN_POINT ( 'NONE',  ( -4.000000000000000000, 2.309401076758498483, -3.433295621305379353 ) ) ;
#12648 = VERTEX_POINT ( 'NONE', #11302 ) ;
#12649 = VERTEX_POINT ( 'NONE', #4673 ) ;
#12650 = DIRECTION ( 'NONE',  ( -1.000000000000000000, -0.000000000000000000, -0.000000000000000000 ) ) ;
#12651 = DIRECTION ( 'NONE',  ( -1.000000000000000000, -0.000000000000000000, -0.000000000000000000 ) ) ;
#12652 = AXIS2_PLACEMENT_3D ( 'NONE', #7045, #9275, #3738 ) ;
#12653 = EDGE_CURVE ( 'NONE', #8972, #1538, #10206, .T. ) ;
#12654 = CARTESIAN_POINT ( 'NONE',  ( 455.5035746174796714, 294.6698471414878782, -187.0000000000000568 ) ) ;
#12655 = VERTEX_POINT ( 'NONE', #8871 ) ;
#12656 = CARTESIAN_POINT ( 'NONE',  ( 650.0000000000000000, 175.0000000000000568, -210.0000000000000000 ) ) ;
#12657 = LINE ( 'NONE', #11629, #8722 ) ;
#12658 = CARTESIAN_POINT ( 'NONE',  ( -1.287237434361707233, -3.875615274277397937, -3.430618716626816500 ) ) ;
#12659 = FACE_OUTER_BOUND ( 'NONE', #1203, .T. ) ;
#12660 = FILL_AREA_STYLE ('',( #4791 ) ) ;
#12661 = VERTEX_POINT ( 'NONE', #5490 ) ;
#12662 = CIRCLE ( 'NONE', #9603, 2.500000000000000888 ) ;
#12663 = DIRECTION ( 'NONE',  ( -1.000000000000000000, 0.000000000000000000, 0.000000000000000000 ) ) ;
#12664 = AXIS2_PLACEMENT_3D ( 'NONE', #3881, #8362, #2750 ) ;
#12665 = VERTEX_POINT ( 'NONE', #13368 ) ;
#12666 = ORIENTED_EDGE ( 'NONE', *, *, #6401, .T. ) ;
#12667 = DIRECTION ( 'NONE',  ( -1.000000000000000000, 0.000000000000000000, 0.000000000000000000 ) ) ;
#12668 = CARTESIAN_POINT ( 'NONE',  ( 145.1678582058265476, 408.6511750828048548, 190.0000000000000000 ) ) ;
#12669 = EDGE_CURVE ( 'NONE', #14275, #14524, #974, .T. ) ;
#12670 = CARTESIAN_POINT ( 'NONE',  ( -6.500000000000000000, -3.752776749732572803, -6.064240316920399998 ) ) ;
#12671 = VECTOR ( 'NONE', #7538, 1000.000000000000000 ) ;
#12672 = CIRCLE ( 'NONE', #4420, 2.700000000000000178 ) ;
#12673 = VERTEX_POINT ( 'NONE', #14488 ) ;
#12674 = CARTESIAN_POINT ( 'NONE',  ( 0.4465819873851995525, 2.886751345948122882, -5.000000000000000000 ) ) ;
#12675 = EDGE_CURVE ( 'NONE', #11084, #3223, #11976, .T. ) ;
#12676 = FACE_OUTER_BOUND ( 'NONE', #12611, .T. ) ;
#12677 = DIRECTION ( 'NONE',  ( -1.000000000000000000, -0.000000000000000000, -0.000000000000000000 ) ) ;
#12678 = LINE ( 'NONE', #9365, #14252 ) ;
#12679 = ORIENTED_EDGE ( 'NONE', *, *, #6128, .F. ) ;
#12680 = ADVANCED_FACE ( 'NONE', ( #14554 ), #5164, .F. ) ;
#12681 = ADVANCED_FACE ( 'NONE', ( #12338 ), #2222, .F. ) ;
#12682 = DIRECTION ( 'NONE',  ( 1.000000000000000000, 0.000000000000000000, 0.000000000000000000 ) ) ;
#12683 = CARTESIAN_POINT ( 'NONE',  ( -6.080745460913608902, 0.5192545390863924082, -1.000000000000000000 ) ) ;
#12684 = ORIENTED_EDGE ( 'NONE', *, *, #3700, .F. ) ;
#12686 = EDGE_CURVE ( 'NONE', #3660, #12301, #13529, .T. ) ;
#12685 = DIRECTION ( 'NONE',  ( -0.000000000000000000, -0.000000000000000000, 1.000000000000000000 ) ) ;
#12687 = AXIS2_PLACEMENT_3D ( 'NONE', #5506, #3148, #1055 ) ;
#12688 = ORIENTED_EDGE ( 'NONE', *, *, #3396, .T. ) ;
#12689 = ORIENTED_EDGE ( 'NONE', *, *, #9885, .T. ) ;
#12690 = DIRECTION ( 'NONE',  ( 1.000000000000000000, 0.000000000000000000, 0.000000000000000000 ) ) ;
#12691 = DIRECTION ( 'NONE',  ( -0.000000000000000000, -0.000000000000000000, -1.000000000000000000 ) ) ;
#12692 = B_SPLINE_CURVE_WITH_KNOTS ( 'NONE', 3,
 ( #8183, #3854, #9237, #13657, #5982, #10483 ),
 .UNSPECIFIED., .F., .F.,
 ( 4, 2, 4 ),
 ( 0.002365888236227995517, 0.003551327329835084114, 0.004736766423442172712 ),
 .UNSPECIFIED. ) ;
#12693 = PLANE ( 'NONE',  #5909 ) ;
#12694 = AXIS2_PLACEMENT_3D ( 'NONE', #7705, #5557, #13311 ) ;
#12695 = VECTOR ( 'NONE', #3874, 1000.000000000000227 ) ;
#12696 = UNCERTAINTY_MEASURE_WITH_UNIT (LENGTH_MEASURE( 1.000000000000000082E-05 ), #9936, 'distance_accuracy_value', 'NONE');
#12697 = DIRECTION ( 'NONE',  ( 0.000000000000000000, 1.000000000000000000, 0.000000000000000000 ) ) ;
#12698 = ORIENTED_EDGE ( 'NONE', *, *, #2474, .F. ) ;
#12699 = EDGE_CURVE ( 'NONE', #7340, #5137, #13973, .T. ) ;
#12700 = EDGE_CURVE ( 'NONE', #9530, #14327, #3467, .T. ) ;
#12701 = CARTESIAN_POINT ( 'NONE',  ( 0.05140428708382614731, 4.819072548984002502, 1.653121499799249161 ) ) ;
#12702 = DIRECTION ( 'NONE',  ( 0.000000000000000000, -1.000000000000000000, 3.344232600703091053E-15 ) ) ;
#12703 = DIRECTION ( 'NONE',  ( 0.000000000000000000, 0.000000000000000000, -1.000000000000000000 ) ) ;
#12704 = CIRCLE ( 'NONE', #5168, 4.199999999999926459 ) ;
#12706 = EDGE_CURVE ( 'NONE', #11363, #14510, #13889, .T. ) ;
#12705 = CARTESIAN_POINT ( 'NONE',  ( 6.452281807715710471, 2.898928808473055341, 5.021091983800445746 ) ) ;
#12707 = ORIENTED_EDGE ( 'NONE', *, *, #13561, .T. ) ;
#12708 = ORIENTED_EDGE ( 'NONE', *, *, #2609, .F. ) ;
#12709 = DIRECTION ( 'NONE',  ( 1.003269780210927276E-15, 3.344232600703091053E-15, -1.000000000000000000 ) ) ;
#12710 = LINE ( 'NONE', #2740, #12013 ) ;
#12711 = AXIS2_PLACEMENT_3D ( 'NONE', #589, #528, #4154 ) ;
#12712 = CIRCLE ( 'NONE', #5880, 2.500000000000000888 ) ;
#12713 = CARTESIAN_POINT ( 'NONE',  ( 1.500000000000001332, 0.000000000000000000, 0.000000000000000000 ) ) ;
#12714 =( GEOMETRIC_REPRESENTATION_CONTEXT ( 3 ) GLOBAL_UNCERTAINTY_ASSIGNED_CONTEXT ( ( #6665 ) ) GLOBAL_UNIT_ASSIGNED_CONTEXT ( ( #8676, #5511, #1807 ) ) REPRESENTATION_CONTEXT ( 'NONE', 'WORKASPACE' ) );
#12715 = VERTEX_POINT ( 'NONE', #2673 ) ;
#12716 = CARTESIAN_POINT ( 'NONE',  ( 8.500000000000000000, 0.000000000000000000, 0.000000000000000000 ) ) ;
#12717 = CARTESIAN_POINT ( 'NONE',  ( -1.149515148933674504E-15, -4.647091401871393579, -3.572172305156879890 ) ) ;
#12718 = FACE_OUTER_BOUND ( 'NONE', #11064, .T. ) ;
#12719 = VECTOR ( 'NONE', #2100, 1000.000000000000000 ) ;
#12720 = AXIS2_PLACEMENT_3D ( 'NONE', #2390, #13318, #4389 ) ;
#12721 = CARTESIAN_POINT ( 'NONE',  ( 611.4942090049451053, 232.4210031920599135, -184.7999999999999829 ) ) ;
#12722 = PLANE ( 'NONE',  #11487 ) ;
#12723 = CARTESIAN_POINT ( 'NONE',  ( -1.269541193505925744E-15, 7.895640089090863789, -6.564402953523717166 ) ) ;
#12724 = ORIENTED_EDGE ( 'NONE', *, *, #12699, .F. ) ;
#12725 = CARTESIAN_POINT ( 'NONE',  ( 4.358513833876415333, 4.989164364209877967, -0.07763482564820642362 ) ) ;
#12726 = ORIENTED_EDGE ( 'NONE', *, *, #9811, .F. ) ;
#12727 = ORIENTED_EDGE ( 'NONE', *, *, #6923, .T. ) ;
#12728 = VECTOR ( 'NONE', #8742, 1000.000000000000114 ) ;
#12729 = CARTESIAN_POINT ( 'NONE',  ( 707.0389973793288618, 162.8315651648156575, -177.6000000000005059 ) ) ;
#12730 = AXIS2_PLACEMENT_3D ( 'NONE', #7638, #13029, #8519 ) ;
#12731 = VECTOR ( 'NONE', #11624, 1000.000000000000000 ) ;
#12732 = VECTOR ( 'NONE', #9786, 1000.000000000000000 ) ;
#12733 = LINE ( 'NONE', #312, #939 ) ;
#12734 = CARTESIAN_POINT ( 'NONE',  ( 704.6332369798501531, 163.5532932846598726, 177.6000000000001648 ) ) ;
#12735 = CARTESIAN_POINT ( 'NONE',  ( -0.1920286436967154065, 8.541911424052788811E-16, -6.975000000000000533 ) ) ;
#12736 = AXIS2_PLACEMENT_3D ( 'NONE', #4435, #12326, #5611 ) ;
#12737 = ORIENTED_EDGE ( 'NONE', *, *, #8983, .F. ) ;
#12738 = FACE_OUTER_BOUND ( 'NONE', #4055, .T. ) ;
#12739 = DIRECTION ( 'NONE',  ( 0.000000000000000000, 0.000000000000000000, -1.000000000000000000 ) ) ;
#12740 = AXIS2_PLACEMENT_3D ( 'NONE', #134, #3417, #9026 ) ;
#12741 = DIRECTION ( 'NONE',  ( 0.000000000000000000, 0.000000000000000000, -1.000000000000000000 ) ) ;
#12742 = DIRECTION ( 'NONE',  ( -0.2873478855663454401, -0.9578262852211514300, 0.000000000000000000 ) ) ;
#12743 = PRESENTATION_STYLE_ASSIGNMENT (( #10522 ) ) ;
#12744 = EDGE_LOOP ( 'NONE', ( #9918, #6419, #81, #2057 ) ) ;
#12745 = AXIS2_PLACEMENT_3D ( 'NONE', #6428, #576, #7386 ) ;
#12746 = VECTOR ( 'NONE', #10538, 1000.000000000000114 ) ;
#12747 = CARTESIAN_POINT ( 'NONE',  ( 3.250000000000004441, 5.629165124598849879, 0.000000000000000000 ) ) ;
#12748 = ORIENTED_EDGE ( 'NONE', *, *, #10710, .T. ) ;
#12749 = EDGE_CURVE ( 'NONE', #12569, #11133, #14035, .T. ) ;
#12750 = ADVANCED_FACE ( 'NONE', ( #11660, #7236, #10488, #1553, #11517, #10341, #12923 ), #7095, .T. ) ;
#12752 = CARTESIAN_POINT ( 'NONE',  ( 601.4378431141739156, -180.4313529342555000, 9.352357694252897163E-13 ) ) ;
#12751 = AXIS2_PLACEMENT_3D ( 'NONE', #3191, #2216, #7628 ) ;
#12753 = AXIS2_PLACEMENT_3D ( 'NONE', #12586, #4625, #9112 ) ;
#12754 = LINE ( 'NONE', #11636, #5425 ) ;
#12755 = CARTESIAN_POINT ( 'NONE',  ( 3.333333333333332593, 2.694301256218250007, -3.300726591567078483 ) ) ;
#12756 = ORIENTED_EDGE ( 'NONE', *, *, #2429, .F. ) ;
#12757 = CARTESIAN_POINT ( 'NONE',  ( 609.7455576527837593, 188.4502455723027481, 189.3436892194421546 ) ) ;
#12758 = DIRECTION ( 'NONE',  ( 1.000000000000000000, 0.000000000000000000, 0.000000000000000000 ) ) ;
#12759 = CARTESIAN_POINT ( 'NONE',  ( 0.05140428708382493994, -3.841181488860375026, 3.346878500200758833 ) ) ;
#12760 = AXIS2_PLACEMENT_3D ( 'NONE', #1086, #5887, #181 ) ;
#12761 = CARTESIAN_POINT ( 'NONE',  ( -0.1756481739660520902, 4.720212674038980261, -3.469390959564065291 ) ) ;
#12762 = ORIENTED_EDGE ( 'NONE', *, *, #1065, .T. ) ;
#12763 = AXIS2_PLACEMENT_3D ( 'NONE', #9609, #8280, #12859 ) ;
#12764 = CARTESIAN_POINT ( 'NONE',  ( 6.445127866599362321, 3.194847394660946804, -4.687657648742338701 ) ) ;
#12765 = EDGE_LOOP ( 'NONE', ( #4121, #2537, #12756, #6988 ) ) ;
#12766 = ADVANCED_FACE ( 'NONE', ( #6140 ), #9316, .T. ) ;
#12767 = DIRECTION ( 'NONE',  ( 0.000000000000000000, 1.224646799147353207E-16, 1.000000000000000000 ) ) ;
#12768 = ORIENTED_EDGE ( 'NONE', *, *, #4137, .F. ) ;
#12769 = EDGE_LOOP ( 'NONE', ( #10821, #8415, #12119, #3171 ) ) ;
#12770 =( LENGTH_UNIT ( ) NAMED_UNIT ( * ) SI_UNIT ( .MILLI., .METRE. ) );
#12771 = DIRECTION ( 'NONE',  ( -0.9578262852211514300, 0.2873478855663452736, -1.110223024625156540E-15 ) ) ;
#12772 = CARTESIAN_POINT ( 'NONE',  ( 6.534533895392293346, -2.951347675328725995, 5.111884124469654900 ) ) ;
#12773 = AXIS2_PLACEMENT_3D ( 'NONE', #7048, #249, #3955 ) ;
#12774 = EDGE_CURVE ( 'NONE', #8156, #12403, #1839, .T. ) ;
#12775 = PRODUCT_DEFINITION_SHAPE ( 'NONE', 'NONE',  #6844 ) ;
#12776 = DIRECTION ( 'NONE',  ( -9.794481010665704304E-16, -3.264827003555233190E-15, -1.000000000000000000 ) ) ;
#12777 = CARTESIAN_POINT ( 'NONE',  ( 0.000000000000000000, -4.330127018922189208, 2.500000000000010658 ) ) ;
#12778 = EDGE_LOOP ( 'NONE', ( #451, #4544, #10111, #9550 ) ) ;
#12779 = FACE_OUTER_BOUND ( 'NONE', #14044, .T. ) ;
#12780 = CARTESIAN_POINT ( 'NONE',  ( -2.000000000000007550, -3.464101615137749945, 0.000000000000000000 ) ) ;
#12781 = CARTESIAN_POINT ( 'NONE',  ( 455.5035746174796145, 294.6698471414878782, 178.5000000000000568 ) ) ;
#12782 = CIRCLE ( 'NONE', #5252, 0.2000000000000000944 ) ;
#12783 = EDGE_CURVE ( 'NONE', #5286, #4296, #7504, .T. ) ;
#12784 = CARTESIAN_POINT ( 'NONE',  ( 6.481779955677544613, 2.910222513313213799, 5.040653254389286353 ) ) ;
#12785 = EDGE_LOOP ( 'NONE', ( #9871, #6192, #5743, #12299 ) ) ;
#12786 = ORIENTED_EDGE ( 'NONE', *, *, #13968, .F. ) ;
#12787 = DIRECTION ( 'NONE',  ( 0.000000000000000000, -1.000000000000000000, 1.314525273895018220E-15 ) ) ;
#12788 = DIRECTION ( 'NONE',  ( -0.000000000000000000, -0.000000000000000000, 1.000000000000000000 ) ) ;
#12789 = DIRECTION ( 'NONE',  ( 9.794481010665704304E-16, 3.264827003555233190E-15, 1.000000000000000000 ) ) ;
#12790 = DIRECTION ( 'NONE',  ( -0.000000000000000000, -0.000000000000000000, 1.000000000000000000 ) ) ;
#12791 = EDGE_CURVE ( 'NONE', #12984, #10586, #3863, .T. ) ;
#12792 = EDGE_CURVE ( 'NONE', #7639, #5487, #289, .T. ) ;
#12793 = CIRCLE ( 'NONE', #12558, 2.200000000000009948 ) ;
#12794 = PLANE ( 'NONE',  #9655 ) ;
#12795 = EDGE_LOOP ( 'NONE', ( #5086, #4640, #4467, #13682 ) ) ;
#12796 = EDGE_CURVE ( 'NONE', #6863, #5856, #12853, .T. ) ;
#12797 = PRODUCT_RELATED_PRODUCT_CATEGORY ( 'part', '', ( #124 ) ) ;
#12798 = DIRECTION ( 'NONE',  ( -0.9578262852211489875, 0.2873478855663534892, 0.000000000000000000 ) ) ;
#12799 = CARTESIAN_POINT ( 'NONE',  ( 610.0000000000001137, 191.1080398579019572, -186.9697000000000173 ) ) ;
#12800 = CARTESIAN_POINT ( 'NONE',  ( 153.1991633467111456, 386.6211705227183870, -187.0000000000000568 ) ) ;
#12801 = B_SPLINE_CURVE_WITH_KNOTS ( 'NONE', 3,
 ( #6228, #13993, #4908, #5195, #11829, #7411 ),
 .UNSPECIFIED., .F., .F.,
 ( 4, 2, 4 ),
 ( 0.01471339550406853582, 0.01588188803547990399, 0.01705038056689127043 ),
 .UNSPECIFIED. ) ;
#12802 = LINE ( 'NONE', #599, #6087 ) ;
#12803 = CARTESIAN_POINT ( 'NONE',  ( 0.000000000000000000, 0.000000000000000000, -25.03750572909317285 ) ) ;
#12804 = DIRECTION ( 'NONE',  ( 0.000000000000000000, 0.000000000000000000, -1.000000000000000000 ) ) ;
#12805 =( NAMED_UNIT ( * ) SI_UNIT ( $, .STERADIAN. ) SOLID_ANGLE_UNIT ( ) );
#12806 = ORIENTED_EDGE ( 'NONE', *, *, #12425, .F. ) ;
#12807 = DIRECTION ( 'NONE',  ( 1.000000000000000000, 0.000000000000000000, 0.000000000000000000 ) ) ;
#12808 = ORIENTED_EDGE ( 'NONE', *, *, #5160, .F. ) ;
#12809 = ORIENTED_EDGE ( 'NONE', *, *, #1602, .F. ) ;
#12810 = AXIS2_PLACEMENT_3D ( 'NONE', #1211, #3367, #14571 ) ;
#12811 = DIRECTION ( 'NONE',  ( -0.2873478855663453846, -0.9578262852211513190, -0.000000000000000000 ) ) ;
#12812 = CARTESIAN_POINT ( 'NONE',  ( 0.000000000000000000, 0.000000000000000000, 0.000000000000000000 ) ) ;
#12813 = FACE_OUTER_BOUND ( 'NONE', #1593, .T. ) ;
#12814 = PLANE ( 'NONE',  #7965 ) ;
#12815 = VERTEX_POINT ( 'NONE', #8343 ) ;
#12816 = FACE_OUTER_BOUND ( 'NONE', #12443, .T. ) ;
#12817 = CARTESIAN_POINT ( 'NONE',  ( 145.1678582058265192, 408.6511750828049117, 210.0000000000000000 ) ) ;
#12818 = FACE_OUTER_BOUND ( 'NONE', #4241, .T. ) ;
#12819 = FACE_OUTER_BOUND ( 'NONE', #8558, .T. ) ;
#12820 = ORIENTED_EDGE ( 'NONE', *, *, #8181, .F. ) ;
#12821 = ADVANCED_FACE ( 'NONE', ( #4890 ), #3709, .F. ) ;
#12822 = CARTESIAN_POINT ( 'NONE',  ( 636.7717819724297215, 155.3244477714206653, -211.0000000000000000 ) ) ;
#12823 = VERTEX_POINT ( 'NONE', #4968 ) ;
#12824 = EDGE_CURVE ( 'NONE', #3430, #4571, #2734, .T. ) ;
#12825 = CARTESIAN_POINT ( 'NONE',  ( 451.6722694765949768, 316.6998517015743460, -210.0000000000000000 ) ) ;
#12826 = APPLICATION_CONTEXT ( 'automotive_design' ) ;
#12827 = CARTESIAN_POINT ( 'NONE',  ( 635.0000000000000000, 160.0000000000000284, 190.0000000000000284 ) ) ;
#12828 = CARTESIAN_POINT ( 'NONE',  ( 227.7315295682384999, 303.4917135554678680, -177.6000000000009038 ) ) ;
#12829 = ORIENTED_EDGE ( 'NONE', *, *, #6731, .F. ) ;
#12830 = CARTESIAN_POINT ( 'NONE',  ( 0.08165819712377203610, -4.939961795957301227, -1.443735181952766400 ) ) ;
#12831 = ADVANCED_FACE ( 'NONE', ( #10642 ), #6339, .F. ) ;
#12832 = EDGE_CURVE ( 'NONE', #1059, #4259, #3796, .T. ) ;
#12833 = CARTESIAN_POINT ( 'NONE',  ( 0.000000000000000000, 0.000000000000000000, -7.974599999999998801 ) ) ;
#12834 = CARTESIAN_POINT ( 'NONE',  ( 6.500000000000000000, 0.6470732608156823940, -0.01945970098673075951 ) ) ;
#12835 = FACE_BOUND ( 'NONE', #1082, .T. ) ;
#12836 = ORIENTED_EDGE ( 'NONE', *, *, #11803, .F. ) ;
#12837 = CARTESIAN_POINT ( 'NONE',  ( 10.00000000000000000, 10.00000000000000178, -190.0000000000000000 ) ) ;
#12838 = CARTESIAN_POINT ( 'NONE',  ( 133.6739427831727198, 370.3381236739588758, 210.0000000000000000 ) ) ;
#12839 = ORIENTED_EDGE ( 'NONE', *, *, #1457, .F. ) ;
#12840 = CARTESIAN_POINT ( 'NONE',  ( 2.999999999999999112, 4.000000000000000000, 0.000000000000000000 ) ) ;
#12841 = VERTEX_POINT ( 'NONE', #14105 ) ;
#12842 = VERTEX_POINT ( 'NONE', #8494 ) ;
#12843 = PLANE ( 'NONE',  #6569 ) ;
#12844 = PLANE ( 'NONE',  #14600 ) ;
#12845 = CARTESIAN_POINT ( 'NONE',  ( 4.197478902586992966, -0.8524102783748346290, -3.505063281295504041 ) ) ;
#12846 = EDGE_CURVE ( 'NONE', #5143, #8855, #1924, .T. ) ;
#12847 = EDGE_CURVE ( 'NONE', #1218, #7610, #3112, .T. ) ;
#12848 = DIRECTION ( 'NONE',  ( 0.000000000000000000, 0.000000000000000000, -1.000000000000000000 ) ) ;
#12849 = UNCERTAINTY_MEASURE_WITH_UNIT (LENGTH_MEASURE( 1.000000000000000082E-05 ), #12118, 'distance_accuracy_value', 'NONE');
#12850 = FACE_OUTER_BOUND ( 'NONE', #9778, .T. ) ;
#12851 = ORIENTED_EDGE ( 'NONE', *, *, #14382, .T. ) ;
#12852 = LINE ( 'NONE', #2672, #3506 ) ;
#12853 = LINE ( 'NONE', #9538, #420 ) ;
#12854 = DIRECTION ( 'NONE',  ( -1.000000000000000000, 0.000000000000000000, 0.000000000000000000 ) ) ;
#12855 = CARTESIAN_POINT ( 'NONE',  ( 137.1540310085880776, 355.9707293956415697, 187.0000000000000000 ) ) ;
#12856 = ORIENTED_EDGE ( 'NONE', *, *, #12495, .T. ) ;
#12857 = ORIENTED_EDGE ( 'NONE', *, *, #698, .F. ) ;
#12858 = DIRECTION ( 'NONE',  ( -1.000000000000000000, 0.000000000000000000, 0.000000000000000000 ) ) ;
#12859 = DIRECTION ( 'NONE',  ( 0.000000000000000000, -0.5000000000000001110, 0.8660254037844387076 ) ) ;
#12860 = CARTESIAN_POINT ( 'NONE',  ( 0.000000000000000000, 0.000000000000000000, 3.469446951953614189E-15 ) ) ;
#12861 = EDGE_CURVE ( 'NONE', #2242, #9111, #3045, .T. ) ;
#12862 = DIRECTION ( 'NONE',  ( -0.000000000000000000, -0.000000000000000000, 1.000000000000000000 ) ) ;
#12863 = ORIENTED_EDGE ( 'NONE', *, *, #7139, .F. ) ;
#12864 = CARTESIAN_POINT ( 'NONE',  ( 451.3035746174797396, 294.6698471414878782, -210.0000000000000000 ) ) ;
#12865 = DIRECTION ( 'NONE',  ( -1.000000000000000000, -0.000000000000000000, -0.000000000000000000 ) ) ;
#12866 = DIRECTION ( 'NONE',  ( -1.000000000000000000, -0.000000000000000000, -0.000000000000000000 ) ) ;
#12867 = EDGE_CURVE ( 'NONE', #12649, #8013, #1842, .T. ) ;
#12868 = DIRECTION ( 'NONE',  ( 0.000000000000000000, 0.000000000000000000, -1.000000000000000000 ) ) ;
#12869 = LINE ( 'NONE', #1568, #6771 ) ;
#12870 = FILL_AREA_STYLE ('',( #3882 ) ) ;
#12871 =( NAMED_UNIT ( * ) PLANE_ANGLE_UNIT ( ) SI_UNIT ( $, .RADIAN. ) );
#12872 = ORIENTED_EDGE ( 'NONE', *, *, #5103, .F. ) ;
#12873 = ADVANCED_FACE ( 'NONE', ( #869 ), #6353, .T. ) ;
#12874 = CARTESIAN_POINT ( 'NONE',  ( 33.05499999999999972, 0.000000000000000000, 0.000000000000000000 ) ) ;
#12875 = ORIENTED_EDGE ( 'NONE', *, *, #12796, .F. ) ;
#12876 = ORIENTED_EDGE ( 'NONE', *, *, #11158, .T. ) ;
#12877 = FACE_OUTER_BOUND ( 'NONE', #15, .T. ) ;
#12878 = EDGE_CURVE ( 'NONE', #9599, #1319, #7532, .T. ) ;
#12879 = FACE_OUTER_BOUND ( 'NONE', #7261, .T. ) ;
#12880 = FACE_OUTER_BOUND ( 'NONE', #11752, .T. ) ;
#12881 = CYLINDRICAL_SURFACE ( 'NONE', #2538, 7.500000000000062172 ) ;
#12882 = ORIENTED_EDGE ( 'NONE', *, *, #14481, .T. ) ;
#12883 = DIRECTION ( 'NONE',  ( -0.2873478855663454401, -0.9578262852211514300, 0.000000000000000000 ) ) ;
#12884 = CARTESIAN_POINT ( 'NONE',  ( 0.000000000000000000, 0.000000000000000000, 0.000000000000000000 ) ) ;
#12885 = LINE ( 'NONE', #14009, #5369 ) ;
#12886 = ORIENTED_EDGE ( 'NONE', *, *, #7774, .F. ) ;
#12887 = EDGE_CURVE ( 'NONE', #5667, #11071, #8792, .T. ) ;
#12888 = ADVANCED_FACE ( 'NONE', ( #1710 ), #14187, .F. ) ;
#12889 = CYLINDRICAL_SURFACE ( 'NONE', #10834, 2.649999999999985700 ) ;
#12890 = CARTESIAN_POINT ( 'NONE',  ( 6.533910050139694725, 2.950514251728030946, -5.110440592449080555 ) ) ;
#12891 = ITEM_DEFINED_TRANSFORMATION ( 'NONE', 'NONE', #5717,  #9440 ) ;
#12892 = ORIENTED_EDGE ( 'NONE', *, *, #6554, .F. ) ;
#12893 = ADVANCED_FACE ( 'NONE', ( #11813 ), #4079, .T. ) ;
#12894 = LINE ( 'NONE', #6107, #10105 ) ;
#12895 = PRODUCT ( 'main frame', 'main frame', '', ( #10033 ) ) ;
#12896 = DIRECTION ( 'NONE',  ( 0.000000000000000000, 1.000000000000000000, 0.000000000000000000 ) ) ;
#12897 = FACE_OUTER_BOUND ( 'NONE', #658, .T. ) ;
#12898 = VERTEX_POINT ( 'NONE', #13003 ) ;
#12899 = CARTESIAN_POINT ( 'NONE',  ( 145.1678582058265192, 408.6511750828049117, -210.0000000000000000 ) ) ;
#12900 = VECTOR ( 'NONE', #3924, 999.9999999999998863 ) ;
#12901 = CONICAL_SURFACE ( 'NONE', #5133, 8.105212085995399107, 1.221730476396037490 ) ;
#12902 = DIRECTION ( 'NONE',  ( -0.000000000000000000, -0.000000000000000000, 1.000000000000000000 ) ) ;
#12903 = LINE ( 'NONE', #8323, #13683 ) ;
#12904 = LINE ( 'NONE', #268, #1220 ) ;
#12905 = VERTEX_POINT ( 'NONE', #5106 ) ;
#12906 = VECTOR ( 'NONE', #579, 1000.000000000000000 ) ;
#12907 = DIRECTION ( 'NONE',  ( -1.000000000000000000, -0.000000000000000000, -0.000000000000000000 ) ) ;
#12908 = FACE_OUTER_BOUND ( 'NONE', #8695, .T. ) ;
#12909 = EDGE_LOOP ( 'NONE', ( #1600, #2480 ) ) ;
#12910 = SHAPE_REPRESENTATION ( 'socket head cap screw_iso_ISO 4762 M5 x 16 - 16N', ( #9440 ), #2396 ) ;
#12911 = ORIENTED_EDGE ( 'NONE', *, *, #10247, .T. ) ;
#12912 = DIRECTION ( 'NONE',  ( 0.000000000000000000, -1.314525273895018220E-15, -1.000000000000000000 ) ) ;
#12913 = CIRCLE ( 'NONE', #3719, 6.080745460913608902 ) ;
#12915 = PLANE ( 'NONE',  #7046 ) ;
#12914 = VECTOR ( 'NONE', #1210, 1000.000000000000000 ) ;
#12916 = FACE_OUTER_BOUND ( 'NONE', #11217, .T. ) ;
#12917 = B_SPLINE_CURVE_WITH_KNOTS ( 'NONE', 3,
 ( #6243, #11911, #2928, #6313, #10742, #613, #2992, #5139, #10815, #7489, #12064, #691, #9720, #1958, #14220, #6469, #4114, #7649 ),
 .UNSPECIFIED., .F., .F.,
 ( 4, 2, 2, 2, 2, 2, 2, 2, 4 ),
 ( 0.000000000000000000, 0.06250000000000000000, 0.1250000000000000000, 0.1875000000000000000, 0.2500000000000000000, 0.3125000000000000000, 0.3750000000000000000, 0.4375000000000000000, 0.5000000000000000000 ),
 .UNSPECIFIED. ) ;
#12918 = FACE_OUTER_BOUND ( 'NONE', #6473, .T. ) ;
#12919 = CARTESIAN_POINT ( 'NONE',  ( 125.3981793592653702, -37.61945380778043102, -182.7999999999979934 ) ) ;
#12920 = VERTEX_POINT ( 'NONE', #8712 ) ;
#12921 = VECTOR ( 'NONE', #7711, 1000.000000000000227 ) ;
#12922 = CARTESIAN_POINT ( 'NONE',  ( 0.3106000600989282101, 5.537975084925940372, 0.4079457818577104100 ) ) ;
#12923 = FACE_BOUND ( 'NONE', #12646, .T. ) ;
#12924 = DIRECTION ( 'NONE',  ( 1.000000000000000000, 0.000000000000000000, 0.000000000000000000 ) ) ;
#12925 = DIRECTION ( 'NONE',  ( -1.000000000000000000, 0.000000000000000000, 0.000000000000000000 ) ) ;
#12926 = ORIENTED_EDGE ( 'NONE', *, *, #12467, .T. ) ;
#12927 = ORIENTED_EDGE ( 'NONE', *, *, #5341, .T. ) ;
#12928 = CARTESIAN_POINT ( 'NONE',  ( 702.5260191523636877, 164.1854586329052097, 150.0000000000013358 ) ) ;
#12929 = FACE_OUTER_BOUND ( 'NONE', #13468, .T. ) ;
#12930 = EDGE_CURVE ( 'NONE', #7999, #2271, #9601, .T. ) ;
#12931 = LINE ( 'NONE', #2906, #13658 ) ;
#12932 = AXIS2_PLACEMENT_3D ( 'NONE', #2483, #9129, #9354 ) ;
#12933 = VECTOR ( 'NONE', #5702, 1000.000000000000000 ) ;
#12934 = AXIS2_PLACEMENT_3D ( 'NONE', #2002, #2152, #6670 ) ;
#12935 = DIRECTION ( 'NONE',  ( 0.000000000000000000, 0.8660254037844380415, -0.5000000000000009992 ) ) ;
#12936 = ORIENTED_EDGE ( 'NONE', *, *, #13790, .F. ) ;
#12937 = DIRECTION ( 'NONE',  ( -0.9578262852211507639, 0.2873478855663477716, 0.000000000000000000 ) ) ;
#12938 = CARTESIAN_POINT ( 'NONE',  ( -0.04050535873993896946, 7.919512791578231514, -6.573129608219091757 ) ) ;
#12939 = LINE ( 'NONE', #14533, #9685 ) ;
#12940 = DIRECTION ( 'NONE',  ( 1.000000000000000000, 0.000000000000000000, -0.000000000000000000 ) ) ;
#12941 = DIRECTION ( 'NONE',  ( 0.000000000000000000, 0.000000000000000000, 1.000000000000000000 ) ) ;
#12942 = CARTESIAN_POINT ( 'NONE',  ( 639.0000000000000000, 156.0000000000000000, -225.5000000000000000 ) ) ;
#12943 = VERTEX_POINT ( 'NONE', #10860 ) ;
#12944 = AXIS2_PLACEMENT_3D ( 'NONE', #12752, #10686, #13053 ) ;
#12945 = CARTESIAN_POINT ( 'NONE',  ( 0.5276280594147412240, -4.314175951381924889, -3.320322319201654881 ) ) ;
#12946 = AXIS2_PLACEMENT_3D ( 'NONE', #4651, #5536, #11286 ) ;
#12947 = VERTEX_POINT ( 'NONE', #5323 ) ;
#12948 = EDGE_LOOP ( 'NONE', ( #14153, #7856, #5915, #3570, #2157, #4277, #1970, #11124 ) ) ;
#12949 = CARTESIAN_POINT ( 'NONE',  ( 2.500000000000000000, 2.357898499370431722, -2.818925648462311528E-15 ) ) ;
#12950 = EDGE_CURVE ( 'NONE', #12598, #10624, #4225, .T. ) ;
#12951 = AXIS2_PLACEMENT_3D ( 'NONE', #8154, #3612, #12663 ) ;
#12952 = DIRECTION ( 'NONE',  ( -0.000000000000000000, -0.000000000000000000, 1.000000000000000000 ) ) ;
#12953 = DIRECTION ( 'NONE',  ( -1.000000000000000000, 0.000000000000000000, 0.000000000000000000 ) ) ;
#12954 = VECTOR ( 'NONE', #6447, 1000.000000000000000 ) ;
#12956 = EDGE_CURVE ( 'NONE', #1135, #4280, #9756, .T. ) ;
#12955 = CARTESIAN_POINT ( 'NONE',  ( 631.0000000000000000, 155.9999999999999432, -233.5000000000000000 ) ) ;
#12957 = VECTOR ( 'NONE', #8839, 1000.000000000000000 ) ;
#12958 = ORIENTED_EDGE ( 'NONE', *, *, #3315, .F. ) ;
#12959 = PLANE ( 'NONE',  #6643 ) ;
#12960 = CARTESIAN_POINT ( 'NONE',  ( 6.815765296784352500, 0.6502800852031724865, -6.170377922158368555 ) ) ;
#12961 = DIRECTION ( 'NONE',  ( 0.000000000000000000, 1.000000000000000000, 0.000000000000000000 ) ) ;
#12962 = CARTESIAN_POINT ( 'NONE',  ( 637.0568832135862749, 155.4426727739092655, 211.0000000000000000 ) ) ;
#12963 =( NAMED_UNIT ( * ) PLANE_ANGLE_UNIT ( ) SI_UNIT ( $, .RADIAN. ) );
#12964 = ORIENTED_EDGE ( 'NONE', *, *, #518, .T. ) ;
#12965 = AXIS2_PLACEMENT_3D ( 'NONE', #10884, #760, #3056 ) ;
#12966 = CARTESIAN_POINT ( 'NONE',  ( 10.00000000000000000, 0.000000000000000000, -190.0000000000000000 ) ) ;
#12967 = VERTEX_POINT ( 'NONE', #14321 ) ;
#12968 = EDGE_CURVE ( 'NONE', #14024, #13548, #8707, .T. ) ;
#12969 = VECTOR ( 'NONE', #11120, 1000.000000000000000 ) ;
#12970 = CONICAL_SURFACE ( 'NONE', #6134, 4.000000000000000000, 1.047197551196600296 ) ;
#12971 = FACE_OUTER_BOUND ( 'NONE', #9096, .T. ) ;
#12972 = CARTESIAN_POINT ( 'NONE',  ( 6.818272094961329799, 1.321852500971154365, -6.208027553811807486 ) ) ;
#12973 = PLANE ( 'NONE',  #7578 ) ;
#12974 = EDGE_CURVE ( 'NONE', #6810, #10436, #10032, .T. ) ;
#12975 = ORIENTED_EDGE ( 'NONE', *, *, #9319, .T. ) ;
#12976 = CARTESIAN_POINT ( 'NONE',  ( -9.498873539028489220E-16, 10.00000000000000000, -190.0000000000000000 ) ) ;
#12977 = AXIS2_PLACEMENT_3D ( 'NONE', #1735, #12952, #2698 ) ;
#12978 = EDGE_CURVE ( 'NONE', #14024, #11464, #399, .T. ) ;
#12979 = VECTOR ( 'NONE', #8290, 1000.000000000000114 ) ;
#12980 = PRODUCT_RELATED_PRODUCT_CATEGORY ( 'part', '', ( #5567 ) ) ;
#12981 = CARTESIAN_POINT ( 'NONE',  ( 610.6325945170714249, 188.6953700521320911, -185.3721572044278787 ) ) ;
#12982 = LINE ( 'NONE', #4943, #12746 ) ;
#12983 = DIRECTION ( 'NONE',  ( -0.000000000000000000, -0.000000000000000000, -1.000000000000000000 ) ) ;
#12984 = VERTEX_POINT ( 'NONE', #3402 ) ;
#12985 = CARTESIAN_POINT ( 'NONE',  ( 6.270568613849415662, 3.932080789230358420, -3.401571648088638433 ) ) ;
#12986 = VERTEX_POINT ( 'NONE', #6781 ) ;
#12987 = VECTOR ( 'NONE', #10769, 1000.000000000000000 ) ;
#12988 = ORIENTED_EDGE ( 'NONE', *, *, #13526, .T. ) ;
#12989 = AXIS2_PLACEMENT_3D ( 'NONE', #8766, #7719, #14365 ) ;
#12990 = ORIENTED_EDGE ( 'NONE', *, *, #5239, .T. ) ;
#12991 = PLANE ( 'NONE',  #8913 ) ;
#12992 = AXIS2_PLACEMENT_3D ( 'NONE', #8703, #5169, #12995 ) ;
#12993 = MECHANICAL_DESIGN_GEOMETRIC_PRESENTATION_REPRESENTATION (  '', ( #12509 ), #5226 ) ;
#12994 = CARTESIAN_POINT ( 'NONE',  ( 139.8040310085880833, 355.9707293956415697, 187.0000000000000000 ) ) ;
#12995 = DIRECTION ( 'NONE',  ( 0.000000000000000000, 0.000000000000000000, 1.000000000000000000 ) ) ;
#12996 = VECTOR ( 'NONE', #5658, 999.9999999999998863 ) ;
#12997 = CARTESIAN_POINT ( 'NONE',  ( 650.0000000000000000, 175.0000000000000568, 210.0000000000000000 ) ) ;
#12998 = VECTOR ( 'NONE', #2680, 1000.000000000000000 ) ;
#12999 = DIRECTION ( 'NONE',  ( 1.000000000000000000, 0.000000000000000000, -0.000000000000000000 ) ) ;
#13000 = ORIENTED_EDGE ( 'NONE', *, *, #3960, .F. ) ;
#13001 = VECTOR ( 'NONE', #844, 1000.000000000000000 ) ;
#13002 = PLANE ( 'NONE',  #3031 ) ;
#13003 = CARTESIAN_POINT ( 'NONE',  ( 640.2500000000000000, 160.0000000000000284, -207.0000000000000000 ) ) ;
#13004 = CARTESIAN_POINT ( 'NONE',  ( 455.5035746174796145, 294.6698471414878782, 218.0000000000000000 ) ) ;
#13005 = CARTESIAN_POINT ( 'NONE',  ( 2.500000000000000000, 1.178949249685217415, 2.041999999999998483 ) ) ;
#13006 = EDGE_CURVE ( 'NONE', #13306, #5999, #12386, .T. ) ;
#13007 = ORIENTED_EDGE ( 'NONE', *, *, #5834, .F. ) ;
#13008 = ORIENTED_EDGE ( 'NONE', *, *, #7887, .T. ) ;
#13009 = AXIS2_PLACEMENT_3D ( 'NONE', #13707, #5797, #3520 ) ;
#13010 = FACE_OUTER_BOUND ( 'NONE', #4929, .T. ) ;
#13011 = CARTESIAN_POINT ( 'NONE',  ( -0.5590169943749470072, 0.000000000000000000, 0.000000000000000000 ) ) ;
#13012 = ADVANCED_FACE ( 'NONE', ( #7963 ), #6716, .T. ) ;
#13013 = FACE_OUTER_BOUND ( 'NONE', #3486, .T. ) ;
#13014 = FACE_OUTER_BOUND ( 'NONE', #8651, .T. ) ;
#13015 = ORIENTED_EDGE ( 'NONE', *, *, #3188, .F. ) ;
#13016 = UNCERTAINTY_MEASURE_WITH_UNIT (LENGTH_MEASURE( 1.000000000000000082E-05 ), #2393, 'distance_accuracy_value', 'NONE');
#13017 = AXIS2_PLACEMENT_3D ( 'NONE', #10317, #13507, #5749 ) ;
#13018 = CARTESIAN_POINT ( 'NONE',  ( -3.250000000000003997, -5.629165124598849879, 0.000000000000000000 ) ) ;
#13019 = DIRECTION ( 'NONE',  ( -0.000000000000000000, -0.000000000000000000, -1.000000000000000000 ) ) ;
#13020 = DIRECTION ( 'NONE',  ( 0.000000000000000000, 0.000000000000000000, -1.000000000000000000 ) ) ;
#13021 = EDGE_CURVE ( 'NONE', #12655, #6440, #9408, .T. ) ;
#13022 = CARTESIAN_POINT ( 'NONE',  ( -2.500000000000000888, 0.000000000000000000, -4.974599999999998801 ) ) ;
#13023 = DIRECTION ( 'NONE',  ( 0.000000000000000000, 1.000000000000000000, 0.000000000000000000 ) ) ;
#13024 = CARTESIAN_POINT ( 'NONE',  ( 0.000000000000000000, 2.357898499370431722, -2.818925648462311528E-15 ) ) ;
#13025 =( NAMED_UNIT ( * ) PLANE_ANGLE_UNIT ( ) SI_UNIT ( $, .RADIAN. ) );
#13026 = PRODUCT_DEFINITION_SHAPE ( 'NONE', 'NONE',  #14631 ) ;
#13027 = EDGE_LOOP ( 'NONE', ( #10773, #10497, #8491 ) ) ;
#13028 = PRODUCT_DEFINITION_FORMATION_WITH_SPECIFIED_SOURCE ( 'ANY', '', #12895, .NOT_KNOWN. ) ;
#13029 = DIRECTION ( 'NONE',  ( 0.000000000000000000, 0.000000000000000000, 1.000000000000000000 ) ) ;
#13030 = ADVANCED_BREP_SHAPE_REPRESENTATION ( '', ( #2645, #9440 ), #5943 ) ;
#13031 = EDGE_LOOP ( 'NONE', ( #4150, #1441, #12178, #560 ) ) ;
#13032 = ORIENTED_EDGE ( 'NONE', *, *, #2151, .F. ) ;
#13033 = CARTESIAN_POINT ( 'NONE',  ( -4.000000000000000000, 0.3987449864459974846, -0.01220643443059782861 ) ) ;
#13034 = VECTOR ( 'NONE', #13448, 1000.000000000000000 ) ;
#13035 = CARTESIAN_POINT ( 'NONE',  ( 639.0000000000000000, 156.0000000000000000, -233.5000000000000000 ) ) ;
#13036 = PLANE ( 'NONE',  #9126 ) ;
#13037 = CARTESIAN_POINT ( 'NONE',  ( 2.500000000000000000, 2.357898499370431722, -2.818925648462311528E-15 ) ) ;
#13038 = PRODUCT ( 'hub', 'hub', '', ( #9971 ) ) ;
#13039 = ORIENTED_EDGE ( 'NONE', *, *, #13297, .F. ) ;
#13040 = CARTESIAN_POINT ( 'NONE',  ( 6.362374563308329734, -5.433808049140088414, 0.8060918076006072797 ) ) ;
#13041 = EDGE_CURVE ( 'NONE', #14011, #9542, #6651, .T. ) ;
#13042 = DIRECTION ( 'NONE',  ( 0.9578262852211513190, -0.2873478855663453291, -0.000000000000000000 ) ) ;
#13043 = CARTESIAN_POINT ( 'NONE',  ( 7.336184427528458230, 0.000000000000000000, 0.000000000000000000 ) ) ;
#13044 = DIRECTION ( 'NONE',  ( -1.000000000000000000, -0.000000000000000000, -0.000000000000000000 ) ) ;
#13045 = SURFACE_SIDE_STYLE ('',( #7714 ) ) ;
#13046 = VECTOR ( 'NONE', #1884, 1000.000000000000000 ) ;
#13047 = EDGE_LOOP ( 'NONE', ( #12615, #13173, #7511, #4995 ) ) ;
#13048 = CARTESIAN_POINT ( 'NONE',  ( -1.400000000000000133, 0.000000000000000000, 0.000000000000000000 ) ) ;
#13049 = CARTESIAN_POINT ( 'NONE',  ( 610.0000000000001137, 191.1080398579018720, 187.0000000000000000 ) ) ;
#13050 = ITEM_DEFINED_TRANSFORMATION ( 'NONE', 'NONE', #5018,  #9440 ) ;
#13051 = B_SPLINE_CURVE_WITH_KNOTS ( 'NONE', 3,
 ( #8376, #548, #5073, #3953, #10739 ),
 .UNSPECIFIED., .F., .F.,
 ( 4, 1, 4 ),
 ( 0.000000000000000000, 0.003752776749732569198, 0.007505553499465138396 ),
 .UNSPECIFIED. ) ;
#13052 = ORIENTED_EDGE ( 'NONE', *, *, #11098, .F. ) ;
#13053 = DIRECTION ( 'NONE',  ( -0.2873478855663502141, -0.9578262852211498757, 0.000000000000000000 ) ) ;
#13054 = CARTESIAN_POINT ( 'NONE',  ( 0.1391502195351409510, 4.241015250120811153, -0.6543461111163325628 ) ) ;
#13055 = DIRECTION ( 'NONE',  ( 0.1305261922200524338, -0.9914448613738102711, 0.000000000000000000 ) ) ;
#13056 = ORIENTED_EDGE ( 'NONE', *, *, #2748, .F. ) ;
#13057 = CARTESIAN_POINT ( 'NONE',  ( 610.0429133068968213, 190.7986032820865319, 186.9697000000000173 ) ) ;
#13058 = ADVANCED_FACE ( 'NONE', ( #10189 ), #2206, .F. ) ;
#13059 = CARTESIAN_POINT ( 'NONE',  ( -8.505790995054992365, 418.4210031920607662, -190.0000000000000000 ) ) ;
#13060 = DIRECTION ( 'NONE',  ( 1.000000000000000000, 0.000000000000000000, 0.000000000000000000 ) ) ;
#13061 = ORIENTED_EDGE ( 'NONE', *, *, #1748, .T. ) ;
#13062 = EDGE_CURVE ( 'NONE', #13338, #5340, #1852, .T. ) ;
#13063 = CARTESIAN_POINT ( 'NONE',  ( -6.499999999999999112, 2.227636940139124722, -0.2900584647821222717 ) ) ;
#13064 = VERTEX_POINT ( 'NONE', #3328 ) ;
#13065 = ADVANCED_FACE ( 'NONE', ( #7834 ), #13884, .T. ) ;
#13066 = ADVANCED_FACE ( 'NONE', ( #6861 ), #2053, .T. ) ;
#13067 = ORIENTED_EDGE ( 'NONE', *, *, #4868, .T. ) ;
#13068 = LINE ( 'NONE', #5166, #12445 ) ;
#13069 = EDGE_CURVE ( 'NONE', #5667, #9054, #3245, .T. ) ;
#13070 = DIRECTION ( 'NONE',  ( 0.000000000000000000, 0.000000000000000000, 1.000000000000000000 ) ) ;
#13071 = LINE ( 'NONE', #10850, #9924 ) ;
#13072 = CARTESIAN_POINT ( 'NONE',  ( -4.211140560182196957, -2.431303136016552013, -3.745885042887436178 ) ) ;
#13073 = CARTESIAN_POINT ( 'NONE',  ( -6.826399921716642005, -2.638123634694629516, -6.344399053232583796 ) ) ;
#13074 = ORIENTED_EDGE ( 'NONE', *, *, #6809, .T. ) ;
#13075 = CARTESIAN_POINT ( 'NONE',  ( 451.6722694765949768, 316.6998517015743460, 210.0000000000000000 ) ) ;
#13076 = DIRECTION ( 'NONE',  ( 0.9578262852211507639, -0.2873478855663477716, 0.000000000000000000 ) ) ;
#13077 =( NAMED_UNIT ( * ) PLANE_ANGLE_UNIT ( ) SI_UNIT ( $, .RADIAN. ) );
#13078 = ADVANCED_FACE ( 'NONE', ( #7754 ), #6805, .T. ) ;
#13079 = ADVANCED_FACE ( 'NONE', ( #1027 ), #619, .F. ) ;
#13080 = DIRECTION ( 'NONE',  ( 0.000000000000000000, -0.5000000000000009992, 0.8660254037844381525 ) ) ;
#13081 = VERTEX_POINT ( 'NONE', #1808 ) ;
#13082 = ORIENTED_EDGE ( 'NONE', *, *, #4008, .F. ) ;
#13083 = DIRECTION ( 'NONE',  ( -0.000000000000000000, -0.000000000000000000, -1.000000000000000000 ) ) ;
#13084 = CARTESIAN_POINT ( 'NONE',  ( 112.9652219749295341, 376.5507399164317803, 210.0000000000000000 ) ) ;
#13085 = CARTESIAN_POINT ( 'NONE',  ( 609.7735223591643035, 188.7684563956151464, -189.4730470240896807 ) ) ;
#13086 = CARTESIAN_POINT ( 'NONE',  ( 2.500000000000000000, -1.178949249685214307, 2.042000000000001592 ) ) ;
#13087 = ORIENTED_EDGE ( 'NONE', *, *, #2590, .F. ) ;
#13088 = EDGE_CURVE ( 'NONE', #11698, #1513, #10683, .T. ) ;
#13089 = DIRECTION ( 'NONE',  ( 0.000000000000000000, 0.000000000000000000, -1.000000000000000000 ) ) ;
#13090 = DIRECTION ( 'NONE',  ( -1.000000000000000000, -0.000000000000000000, -0.000000000000000000 ) ) ;
#13091 = DIRECTION ( 'NONE',  ( 0.000000000000000000, 0.000000000000000000, -1.000000000000000000 ) ) ;
#13092 = ORIENTED_EDGE ( 'NONE', *, *, #9626, .F. ) ;
#13093 = DIRECTION ( 'NONE',  ( 0.000000000000000000, 0.000000000000000000, -1.000000000000000000 ) ) ;
#13094 = CARTESIAN_POINT ( 'NONE',  ( 1.567478505476134606E-15, 4.618802153517012066, -3.433295621305382905 ) ) ;
#13095 = DIRECTION ( 'NONE',  ( 0.1305261922200524616, 0.9914448613738103822, -0.000000000000000000 ) ) ;
#13096 = ORIENTED_EDGE ( 'NONE', *, *, #4848, .T. ) ;
#13097 = DIRECTION ( 'NONE',  ( -1.000000000000000000, -0.000000000000000000, -0.000000000000000000 ) ) ;
#13098 = VERTEX_POINT ( 'NONE', #3626 ) ;
#13099 = ORIENTED_EDGE ( 'NONE', *, *, #13249, .T. ) ;
#13100 = LINE ( 'NONE', #4242, #12728 ) ;
#13101 = DIRECTION ( 'NONE',  ( -0.000000000000000000, -0.000000000000000000, -1.000000000000000000 ) ) ;
#13102 = ORIENTED_EDGE ( 'NONE', *, *, #5130, .F. ) ;
#13103 = EDGE_LOOP ( 'NONE', ( #2395, #1195, #6892, #9728 ) ) ;
#13104 = CARTESIAN_POINT ( 'NONE',  ( 448.9584422793565750, 264.0194060144110608, -190.0000000000000000 ) ) ;
#13105 =( REPRESENTATION_RELATIONSHIP ('NONE','NONE', #2822, #5290 ) REPRESENTATION_RELATIONSHIP_WITH_TRANSFORMATION ( #7684 )SHAPE_REPRESENTATION_RELATIONSHIP( ) );
#13106 = CARTESIAN_POINT ( 'NONE',  ( 145.1678582058265192, 408.6511750828049117, -210.0000000000000000 ) ) ;
#13107 = LINE ( 'NONE', #6534, #644 ) ;
#13108 = CARTESIAN_POINT ( 'NONE',  ( 642.5000000000001137, 160.0000000000000284, -225.5000000000000000 ) ) ;
#13109 = EDGE_LOOP ( 'NONE', ( #8683, #10531, #9590, #3528 ) ) ;
#13110 =( NAMED_UNIT ( * ) SI_UNIT ( $, .STERADIAN. ) SOLID_ANGLE_UNIT ( ) );
#13111 = DIRECTION ( 'NONE',  ( 1.000000000000000000, 0.000000000000000000, 0.000000000000000000 ) ) ;
#13112 = EDGE_LOOP ( 'NONE', ( #8069, #11316, #770, #3311 ) ) ;
#13113 = DIRECTION ( 'NONE',  ( 0.000000000000000000, 0.000000000000000000, -1.000000000000000000 ) ) ;
#13114 = VERTEX_POINT ( 'NONE', #9649 ) ;
#13115 = EDGE_CURVE ( 'NONE', #2433, #4822, #192, .T. ) ;
#13116 = CARTESIAN_POINT ( 'NONE',  ( -6.663120783604506769, 3.846954578057049545, -6.460786012260013145 ) ) ;
#13117 = DIRECTION ( 'NONE',  ( -1.000000000000000000, 0.000000000000000000, 0.000000000000000000 ) ) ;
#13118 = ORIENTED_EDGE ( 'NONE', *, *, #10230, .T. ) ;
#13119 = CARTESIAN_POINT ( 'NONE',  ( 0.000000000000000000, 0.000000000000000000, -7.974599999999998801 ) ) ;
#13120 = CARTESIAN_POINT ( 'NONE',  ( 455.5035746174796714, 294.6698471414878782, -210.0000000000000000 ) ) ;
#13121 = FACE_OUTER_BOUND ( 'NONE', #14506, .T. ) ;
#13122 = SURFACE_SIDE_STYLE ('',( #8618 ) ) ;
#13123 = ORIENTED_EDGE ( 'NONE', *, *, #4950, .F. ) ;
#13124 = SURFACE_STYLE_FILL_AREA ( #12217 ) ;
#13125 = CARTESIAN_POINT ( 'NONE',  ( -6.500000000000000000, 0.3213925021621126255, 6.556035011748282652E-16 ) ) ;
#13126 = VERTEX_POINT ( 'NONE', #13735 ) ;
#13127 = EDGE_LOOP ( 'NONE', ( #9783, #9296, #14018, #11760 ) ) ;
#13128 = DIRECTION ( 'NONE',  ( 0.000000000000000000, 1.000000000000000000, -1.314525273895018220E-15 ) ) ;
#13129 = ADVANCED_FACE ( 'NONE', ( #8110 ), #11751, .T. ) ;
#13130 = CARTESIAN_POINT ( 'NONE',  ( 9.356499856268396542E-16, -7.550815748621849011, -6.286450516131055544 ) ) ;
#13131 = ADVANCED_FACE ( 'NONE', ( #9227 ), #14013, .F. ) ;
#13132 = CARTESIAN_POINT ( 'NONE',  ( 1.500000000000000888, 0.000000000000000000, -5.100000000000000533 ) ) ;
#13133 = VECTOR ( 'NONE', #7811, 1000.000000000000000 ) ;
#13134 = PRODUCT_DEFINITION_SHAPE ( 'NONE', 'NONE',  #14627 ) ;
#13135 = DIRECTION ( 'NONE',  ( -0.000000000000000000, -0.000000000000000000, -1.000000000000000000 ) ) ;
#13136 = EDGE_CURVE ( 'NONE', #11200, #2870, #6066, .T. ) ;
#13137 = PRODUCT_DEFINITION_CONTEXT ( 'detailed design', #14332, 'design' ) ;
#13138 = DIRECTION ( 'NONE',  ( -1.000000000000000000, -0.000000000000000000, -0.000000000000000000 ) ) ;
#13139 = ORIENTED_EDGE ( 'NONE', *, *, #4768, .F. ) ;
#13140 = EDGE_CURVE ( 'NONE', #10347, #5692, #2496, .T. ) ;
#13141 = FACE_OUTER_BOUND ( 'NONE', #1176, .T. ) ;
#13142 = DIRECTION ( 'NONE',  ( 0.000000000000000000, 0.000000000000000000, -1.000000000000000000 ) ) ;
#13143 =( GEOMETRIC_REPRESENTATION_CONTEXT ( 3 ) GLOBAL_UNCERTAINTY_ASSIGNED_CONTEXT ( ( #4598 ) ) GLOBAL_UNIT_ASSIGNED_CONTEXT ( ( #14243, #6336, #4064 ) ) REPRESENTATION_CONTEXT ( 'NONE', 'WORKASPACE' ) );
#13144 = LINE ( 'NONE', #13221, #12024 ) ;
#13145 = CIRCLE ( 'NONE', #14095, 2.649999999999985700 ) ;
#13146 = ORIENTED_EDGE ( 'NONE', *, *, #7541, .T. ) ;
#13147 = VERTEX_POINT ( 'NONE', #4044 ) ;
#13148 = FACE_OUTER_BOUND ( 'NONE', #14572, .T. ) ;
#13149 = CARTESIAN_POINT ( 'NONE',  ( 610.0000000000000000, 10.00000000000005507, -210.0020000000000095 ) ) ;
#13150 = VECTOR ( 'NONE', #2219, 1000.000000000000114 ) ;
#13151 = DIRECTION ( 'NONE',  ( -0.9396926207859138680, 0.000000000000000000, -0.3420201433256536139 ) ) ;
#13152 = CARTESIAN_POINT ( 'NONE',  ( 627.2408731339805854, 284.9098836221799615, -190.0000000000001990 ) ) ;
#13153 = ORIENTED_EDGE ( 'NONE', *, *, #1577, .F. ) ;
#13154 = EDGE_CURVE ( 'NONE', #3784, #12984, #4478, .T. ) ;
#13155 = VECTOR ( 'NONE', #6004, 1000.000000000000000 ) ;
#13156 = DIRECTION ( 'NONE',  ( -0.7071067811865474617, 0.000000000000000000, 0.7071067811865474617 ) ) ;
#13157 = ORIENTED_EDGE ( 'NONE', *, *, #3175, .T. ) ;
#13158 = EDGE_CURVE ( 'NONE', #2989, #7099, #14074, .T. ) ;
#13159 = CARTESIAN_POINT ( 'NONE',  ( 627.2408731339806991, 284.9098836221797342, 190.0000000000001990 ) ) ;
#13160 = CARTESIAN_POINT ( 'NONE',  ( 629.0000000000000000, 154.0000000000000284, 187.5000000000000000 ) ) ;
#13161 = CARTESIAN_POINT ( 'NONE',  ( 3.309651814758565180, -5.455921364805393026, -1.000000000000000000 ) ) ;
#13162 =( NAMED_UNIT ( * ) SI_UNIT ( $, .STERADIAN. ) SOLID_ANGLE_UNIT ( ) );
#13163 = ORIENTED_EDGE ( 'NONE', *, *, #14466, .T. ) ;
#13164 = DIRECTION ( 'NONE',  ( 0.2873478855663315068, 0.9578262852211555378, 0.000000000000000000 ) ) ;
#13165 = ORIENTED_EDGE ( 'NONE', *, *, #14561, .F. ) ;
#13166 = ORIENTED_EDGE ( 'NONE', *, *, #873, .T. ) ;
#13167 = DIRECTION ( 'NONE',  ( 0.000000000000000000, 0.000000000000000000, -1.000000000000000000 ) ) ;
#13168 = VECTOR ( 'NONE', #6848, 1000.000000000000227 ) ;
#13169 = AXIS2_PLACEMENT_3D ( 'NONE', #10880, #8656, #2071 ) ;
#13170 = VECTOR ( 'NONE', #7682, 1000.000000000000114 ) ;
#13171 = LINE ( 'NONE', #3063, #8974 ) ;
#13172 = ORIENTED_EDGE ( 'NONE', *, *, #9632, .T. ) ;
#13173 = ORIENTED_EDGE ( 'NONE', *, *, #10687, .F. ) ;
#13174 = CARTESIAN_POINT ( 'NONE',  ( 716.7018481736364492, 193.3416907550361543, -182.8000000000001819 ) ) ;
#13175 = CARTESIAN_POINT ( 'NONE',  ( 6.838249506730350369, 3.995160516047499222, -6.573190279698081895 ) ) ;
#13176 = AXIS2_PLACEMENT_3D ( 'NONE', #7642, #7143, #6027 ) ;
#13177 = AXIS2_PLACEMENT_3D ( 'NONE', #12165, #13288, #7683 ) ;
#13178 = DIRECTION ( 'NONE',  ( 0.9578262852211513190, -0.2873478855663454401, -1.972152263052529514E-31 ) ) ;
#13179 = LINE ( 'NONE', #693, #9020 ) ;
#13180 =( NAMED_UNIT ( * ) SI_UNIT ( $, .STERADIAN. ) SOLID_ANGLE_UNIT ( ) );
#13181 = ORIENTED_EDGE ( 'NONE', *, *, #10009, .T. ) ;
#13182 = DIRECTION ( 'NONE',  ( -0.2873478855663534892, -0.9578262852211489875, 0.000000000000000000 ) ) ;
#13183 = EDGE_LOOP ( 'NONE', ( #11972, #13061, #5152, #12666 ) ) ;
#13184 = CARTESIAN_POINT ( 'NONE',  ( 164.3243839102495656, 402.9042173714779551, -210.0000000000000000 ) ) ;
#13185 = MECHANICAL_DESIGN_GEOMETRIC_PRESENTATION_REPRESENTATION (  '', ( #7761 ), #8702 ) ;
#13186 = ORIENTED_EDGE ( 'NONE', *, *, #13694, .T. ) ;
#13187 = VECTOR ( 'NONE', #6722, 1000.000000000000000 ) ;
#13188 = VECTOR ( 'NONE', #2251, 999.9999999999998863 ) ;
#13189 = DIRECTION ( 'NONE',  ( 1.000000000000000000, 0.000000000000000000, 0.000000000000000000 ) ) ;
#13190 = EDGE_LOOP ( 'NONE', ( #476, #3886 ) ) ;
#13191 = LINE ( 'NONE', #12149, #9474 ) ;
#13192 = FACE_OUTER_BOUND ( 'NONE', #12053, .T. ) ;
#13193 = CIRCLE ( 'NONE', #9661, 8.542937654374687995 ) ;
#13194 = DIRECTION ( 'NONE',  ( 1.000000000000000000, 0.000000000000000000, 0.000000000000000000 ) ) ;
#13195 = SURFACE_SIDE_STYLE ('',( #13275 ) ) ;
#13196 = ADVANCED_FACE ( 'NONE', ( #7357 ), #8677, .T. ) ;
#13197 = EDGE_LOOP ( 'NONE', ( #13067, #12073, #2774, #4896, #11166, #3440, #12202, #6081, #3496, #13621, #12284, #14492, #12316, #6042, #10007, #13494 ) ) ;
#13198 = VECTOR ( 'NONE', #7144, 1000.000000000000000 ) ;
#13199 = VECTOR ( 'NONE', #7573, 1000.000000000000000 ) ;
#13201 = EDGE_CURVE ( 'NONE', #13316, #11071, #8698, .T. ) ;
#13200 = CARTESIAN_POINT ( 'NONE',  ( 6.270568613849413886, 4.911887854652841057, 1.704496029161937320 ) ) ;
#13202 = SURFACE_STYLE_FILL_AREA ( #719 ) ;
#13203 = ORIENTED_EDGE ( 'NONE', *, *, #2101, .T. ) ;
#13204 = EDGE_LOOP ( 'NONE', ( #7030, #5332, #7918, #4949 ) ) ;
#13206 = DIRECTION ( 'NONE',  ( -0.8660254037844377084, -0.5000000000000015543, 0.000000000000000000 ) ) ;
#13205 = VECTOR ( 'NONE', #1239, 1000.000000000000000 ) ;
#13207 = AXIS2_PLACEMENT_3D ( 'NONE', #6380, #13097, #13244 ) ;
#13208 = PLANE ( 'NONE',  #929 ) ;
#13209 = DIRECTION ( 'NONE',  ( 0.000000000000000000, -1.000000000000000000, 0.000000000000000000 ) ) ;
#13210 = COLOUR_RGB ( '',0.8941176470588234615, 0.8941176470588234615, 0.8941176470588234615 ) ;
#13211 = DIRECTION ( 'NONE',  ( -0.000000000000000000, 0.000000000000000000, 1.000000000000000000 ) ) ;
#13212 = AXIS2_PLACEMENT_3D ( 'NONE', #10429, #3870, #8351 ) ;
#13213 = DIRECTION ( 'NONE',  ( -1.000000000000000000, 0.000000000000000000, 0.000000000000000000 ) ) ;
#13214 = ADVANCED_FACE ( 'NONE', ( #1889 ), #779, .F. ) ;
#13215 = ORIENTED_EDGE ( 'NONE', *, *, #11675, .T. ) ;
#13216 = AXIS2_PLACEMENT_3D ( 'NONE', #12167, #12789, #2055 ) ;
#13217 = DIRECTION ( 'NONE',  ( 0.000000000000000000, 0.000000000000000000, -1.000000000000000000 ) ) ;
#13218 = CARTESIAN_POINT ( 'NONE',  ( 6.445127866599366762, -5.657054305385778470, -0.4229901806197434722 ) ) ;
#13219 = CARTESIAN_POINT ( 'NONE',  ( 148.9991633467111569, 386.6211705227183870, 218.0000000000000000 ) ) ;
#13220 = AXIS2_PLACEMENT_3D ( 'NONE', #10927, #14097, #799 ) ;
#13221 = CARTESIAN_POINT ( 'NONE',  ( 145.1678582058265192, 408.6511750828049117, -210.0000000000000000 ) ) ;
#13222 = ORIENTED_EDGE ( 'NONE', *, *, #5745, .F. ) ;
#13223 = ORIENTED_EDGE ( 'NONE', *, *, #1011, .F. ) ;
#13224 = LINE ( 'NONE', #2059, #9614 ) ;
#13225 = CARTESIAN_POINT ( 'NONE',  ( -5.441945782601304238, -4.363644636964928658, -0.3576316571898465746 ) ) ;
#13226 = ADVANCED_FACE ( 'NONE', ( #12071 ), #5357, .T. ) ;
#13227 = CARTESIAN_POINT ( 'NONE',  ( 609.6994022290995190, 186.4862707338506311, -187.4054488658613593 ) ) ;
#13228 = VECTOR ( 'NONE', #12470, 1000.000000000000000 ) ;
#13229 = AXIS2_PLACEMENT_3D ( 'NONE', #4782, #5725, #3434 ) ;
#13230 = DIRECTION ( 'NONE',  ( -0.000000000000000000, -0.000000000000000000, -1.000000000000000000 ) ) ;
#13231 = AXIS2_PLACEMENT_3D ( 'NONE', #1070, #14517, #4404 ) ;
#13232 = VERTEX_POINT ( 'NONE', #7495 ) ;
#13233 = B_SPLINE_CURVE_WITH_KNOTS ( 'NONE', 3,
 ( #500, #8247, #13948, #12759, #3842, #11864, #6118, #1536 ),
 .UNSPECIFIED., .F., .F.,
 ( 4, 2, 2, 4 ),
 ( 0.002921158011986728538, 0.003648658599403080925, 0.004376159186819432445, 0.005831160361652135485 ),
 .UNSPECIFIED. ) ;
#13234 = DIRECTION ( 'NONE',  ( -0.9578262852211514300, 0.2873478855663454401, 0.000000000000000000 ) ) ;
#13235 = EDGE_CURVE ( 'NONE', #7340, #3596, #10964, .T. ) ;
#13236 = EDGE_LOOP ( 'NONE', ( #7399, #9703 ) ) ;
#13237 = FACE_OUTER_BOUND ( 'NONE', #3275, .T. ) ;
#13238 = CARTESIAN_POINT ( 'NONE',  ( 3.783380760145018981E-16, -7.895640089090872671, -6.564402953523720718 ) ) ;
#13239 = PLANE ( 'NONE',  #2796 ) ;
#13240 =( LENGTH_UNIT ( ) NAMED_UNIT ( * ) SI_UNIT ( .MILLI., .METRE. ) );
#13241 = AXIS2_PLACEMENT_3D ( 'NONE', #2032, #6547, #2940 ) ;
#13242 = ORIENTED_EDGE ( 'NONE', *, *, #647, .T. ) ;
#13243 = AXIS2_PLACEMENT_3D ( 'NONE', #12123, #4168, #5204 ) ;
#13244 = DIRECTION ( 'NONE',  ( 0.000000000000000000, 0.000000000000000000, 1.000000000000000000 ) ) ;
#13245 = EDGE_LOOP ( 'NONE', ( #10397, #3844, #831, #14261 ) ) ;
#13246 = VERTEX_POINT ( 'NONE', #5296 ) ;
#13247 = EDGE_CURVE ( 'NONE', #5414, #8268, #679, .T. ) ;
#13248 = CARTESIAN_POINT ( 'NONE',  ( 10.00000000000000000, 0.000000000000000000, -210.0000000000000000 ) ) ;
#13249 = EDGE_CURVE ( 'NONE', #796, #12967, #13646, .T. ) ;
#13250 =( GEOMETRIC_REPRESENTATION_CONTEXT ( 3 ) GLOBAL_UNCERTAINTY_ASSIGNED_CONTEXT ( ( #4752 ) ) GLOBAL_UNIT_ASSIGNED_CONTEXT ( ( #12400, #6591, #1190 ) ) REPRESENTATION_CONTEXT ( 'NONE', 'WORKASPACE' ) );
#13251 = EDGE_CURVE ( 'NONE', #7242, #13261, #6151, .T. ) ;
#13252 = LINE ( 'NONE', #6464, #10632 ) ;
#13253 = ORIENTED_EDGE ( 'NONE', *, *, #6129, .T. ) ;
#13254 = ORIENTED_EDGE ( 'NONE', *, *, #8085, .T. ) ;
#13255 = CARTESIAN_POINT ( 'NONE',  ( 6.541171661047877173, -5.920857802016178617, -0.02973393389964841538 ) ) ;
#13256 = CARTESIAN_POINT ( 'NONE',  ( 610.0000000000000000, 227.4403065089105951, 190.0000000000000000 ) ) ;
#13257 = AXIS2_PLACEMENT_3D ( 'NONE', #5416, #9917, #14424 ) ;
#13258 = CARTESIAN_POINT ( 'NONE',  ( 0.000000000000000000, 3.464101615137751278, -2.000000000000006217 ) ) ;
#13259 = DIRECTION ( 'NONE',  ( -0.9578262852211498757, 0.2873478855663503251, -1.198990317802636355E-15 ) ) ;
#13260 = DIRECTION ( 'NONE',  ( -9.794481010665704304E-16, -3.264827003555233190E-15, -1.000000000000000000 ) ) ;
#13261 = VERTEX_POINT ( 'NONE', #8355 ) ;
#13262 = DIRECTION ( 'NONE',  ( 0.000000000000000000, 0.000000000000000000, 1.000000000000000000 ) ) ;
#13263 = ORIENTED_EDGE ( 'NONE', *, *, #10722, .T. ) ;
#13264 = VECTOR ( 'NONE', #334, 1000.000000000000000 ) ;
#13265 = CARTESIAN_POINT ( 'NONE',  ( 628.0000000000000000, 152.9999999999999147, -233.5000000000000000 ) ) ;
#13266 = EDGE_LOOP ( 'NONE', ( #3551, #5560, #3134, #9957 ) ) ;
#13267 = DIRECTION ( 'NONE',  ( 0.000000000000000000, 0.000000000000000000, -1.000000000000000000 ) ) ;
#13268 = DIRECTION ( 'NONE',  ( 0.000000000000000000, 0.4999999999999990008, -0.8660254037844391517 ) ) ;
#13269 = AXIS2_PLACEMENT_3D ( 'NONE', #14072, #3958, #14147 ) ;
#13270 = ORIENTED_EDGE ( 'NONE', *, *, #12601, .T. ) ;
#13271 = DIRECTION ( 'NONE',  ( 1.000000000000000000, 0.000000000000000000, 0.000000000000000000 ) ) ;
#13272 = CARTESIAN_POINT ( 'NONE',  ( 0.000000000000000000, 2.357898499370431722, -2.818925648462311528E-15 ) ) ;
#13273 = ADVANCED_FACE ( 'NONE', ( #9768 ), #1721, .T. ) ;
#13274 = PLANE ( 'NONE',  #14216 ) ;
#13275 = SURFACE_STYLE_FILL_AREA ( #5242 ) ;
#13276 = VERTEX_POINT ( 'NONE', #2970 ) ;
#13277 = ADVANCED_FACE ( 'NONE', ( #10653, #9696 ), #12794, .F. ) ;
#13278 = ORIENTED_EDGE ( 'NONE', *, *, #2590, .T. ) ;
#13279 = VERTEX_POINT ( 'NONE', #11891 ) ;
#13280 = AXIS2_PLACEMENT_3D ( 'NONE', #7576, #12066, #836 ) ;
#13281 = CARTESIAN_POINT ( 'NONE',  ( 0.8808064505790902388, -6.997019658119350005, -5.875704392893848826 ) ) ;
#13282 = CARTESIAN_POINT ( 'NONE',  ( 627.5000000000000000, 159.0056981173382553, -209.9999999999999716 ) ) ;
#13283 = CARTESIAN_POINT ( 'NONE',  ( 1.399999999999998579, 0.000000000000000000, -7.500000000000000000 ) ) ;
#13284 = DIRECTION ( 'NONE',  ( 1.000000000000000000, 0.000000000000000000, 0.000000000000000000 ) ) ;
#13285 = LINE ( 'NONE', #2957, #3474 ) ;
#13286 = ORIENTED_EDGE ( 'NONE', *, *, #106, .T. ) ;
#13287 = DIRECTION ( 'NONE',  ( 1.000000000000000000, 0.000000000000000000, 0.000000000000000000 ) ) ;
#13288 = DIRECTION ( 'NONE',  ( -1.000000000000000000, -0.000000000000000000, -0.000000000000000000 ) ) ;
#13289 = APPLICATION_PROTOCOL_DEFINITION ( 'draft international standard', 'automotive_design', 1998, #13570 ) ;
#13290 = B_SPLINE_CURVE_WITH_KNOTS ( 'NONE', 3,
 ( #7069, #6991, #9293, #11360, #11491, #5971 ),
 .UNSPECIFIED., .F., .F.,
 ( 4, 2, 4 ),
 ( 0.005511122051665409173, 0.007432374760074394321, 0.009353627468483380336 ),
 .UNSPECIFIED. ) ;
#13291 = CARTESIAN_POINT ( 'NONE',  ( 610.0000000000000000, 0.000000000000000000, 210.0000000000000000 ) ) ;
#13292 = ORIENTED_EDGE ( 'NONE', *, *, #7111, .T. ) ;
#13293 = EDGE_LOOP ( 'NONE', ( #11643, #10020, #12331, #11765 ) ) ;
#13294 = SURFACE_SIDE_STYLE ('',( #11073 ) ) ;
#13295 = DIRECTION ( 'NONE',  ( -0.2873478855663453291, -0.9578262852211513190, -0.000000000000000000 ) ) ;
#13296 = DIRECTION ( 'NONE',  ( -0.000000000000000000, -0.000000000000000000, -1.000000000000000000 ) ) ;
#13297 = EDGE_CURVE ( 'NONE', #7000, #14483, #3281, .T. ) ;
#13298 = CARTESIAN_POINT ( 'NONE',  ( 3.500000000000000000, 4.618802153517012954, 6.505213034913018715E-16 ) ) ;
#13299 = EDGE_LOOP ( 'NONE', ( #4921, #7558, #1533, #1024, #4035, #5344 ) ) ;
#13300 = CARTESIAN_POINT ( 'NONE',  ( -6.500000000000001776, -2.692912473542373952, -6.218066308278946686 ) ) ;
#13301 = VERTEX_POINT ( 'NONE', #11737 ) ;
#13302 = CARTESIAN_POINT ( 'NONE',  ( 635.0000000000000000, 160.0000000000000284, -222.5000000000000000 ) ) ;
#13303 = PLANE ( 'NONE',  #3513 ) ;
#13304 = FACE_OUTER_BOUND ( 'NONE', #5964, .T. ) ;
#13305 =( LENGTH_UNIT ( ) NAMED_UNIT ( * ) SI_UNIT ( .MILLI., .METRE. ) );
#13306 = VERTEX_POINT ( 'NONE', #6366 ) ;
#13307 = CARTESIAN_POINT ( 'NONE',  ( 0.000000000000000000, 0.5192545390863916310, -1.000000000000000000 ) ) ;
#13308 = ORIENTED_EDGE ( 'NONE', *, *, #5215, .T. ) ;
#13309 = ORIENTED_EDGE ( 'NONE', *, *, #12783, .F. ) ;
#13310 = CARTESIAN_POINT ( 'NONE',  ( 610.0000000000001137, 227.4403065089106235, 190.0000000000000000 ) ) ;
#13311 = DIRECTION ( 'NONE',  ( 0.000000000000000000, 0.000000000000000000, 1.000000000000000000 ) ) ;
#13312 = ADVANCED_FACE ( 'NONE', ( #2684 ), #9480, .T. ) ;
#13313 = DIRECTION ( 'NONE',  ( 0.000000000000000000, 0.000000000000000000, -1.000000000000000000 ) ) ;
#13314 = ADVANCED_FACE ( 'NONE', ( #11670 ), #13659, .T. ) ;
#13315 = ORIENTED_EDGE ( 'NONE', *, *, #6573, .F. ) ;
#13316 = VERTEX_POINT ( 'NONE', #10721 ) ;
#13317 = CARTESIAN_POINT ( 'NONE',  ( 6.095473853218515536, -4.853892138986623195, 1.592812200815997725 ) ) ;
#13318 = DIRECTION ( 'NONE',  ( -9.498873539028489960E-17, 1.000000000000000000, 0.000000000000000000 ) ) ;
#13319 = ADVANCED_FACE ( 'NONE', ( #13014 ), #4979, .T. ) ;
#13320 = DIRECTION ( 'NONE',  ( 0.000000000000000000, 1.000000000000000000, 0.000000000000000000 ) ) ;
#13321 = LINE ( 'NONE', #9852, #9847 ) ;
#13322 = CARTESIAN_POINT ( 'NONE',  ( 3.500000000000000000, 0.000000000000000000, 4.000000000000000000 ) ) ;
#13323 = ORIENTED_EDGE ( 'NONE', *, *, #5920, .T. ) ;
#13324 = ADVANCED_FACE ( 'NONE', ( #7404 ), #13984, .T. ) ;
#13325 = CARTESIAN_POINT ( 'NONE',  ( 609.9288325809317257, 190.4177448864037956, 189.9663414180174925 ) ) ;
#13326 = ITEM_DEFINED_TRANSFORMATION ( 'NONE', 'NONE', #4302,  #9440 ) ;
#13327 = ORIENTED_EDGE ( 'NONE', *, *, #4390, .T. ) ;
#13328 = DIRECTION ( 'NONE',  ( -0.9396926207859143121, 0.000000000000000000, -0.3420201433256525592 ) ) ;
#13329 = ORIENTED_EDGE ( 'NONE', *, *, #6048, .T. ) ;
#13330 = CARTESIAN_POINT ( 'NONE',  ( 0.000000000000000000, 0.000000000000000000, 0.000000000000000000 ) ) ;
#13331 = FACE_OUTER_BOUND ( 'NONE', #12137, .T. ) ;
#13332 = ORIENTED_EDGE ( 'NONE', *, *, #5215, .F. ) ;
#13333 = DIRECTION ( 'NONE',  ( -0.000000000000000000, 0.000000000000000000, -1.000000000000000000 ) ) ;
#13334 = DIRECTION ( 'NONE',  ( -1.000000000000000000, -0.000000000000000000, -0.000000000000000000 ) ) ;
#13335 = ADVANCED_FACE ( 'NONE', ( #8505 ), #1639, .F. ) ;
#13336 = EDGE_CURVE ( 'NONE', #4733, #12153, #7776, .T. ) ;
#13337 = PLANE ( 'NONE',  #13975 ) ;
#13338 = VERTEX_POINT ( 'NONE', #592 ) ;
#13339 = EDGE_CURVE ( 'NONE', #6009, #3508, #14197, .T. ) ;
#13340 = FILL_AREA_STYLE_COLOUR ( '', #14121 ) ;
#13341 = ORIENTED_EDGE ( 'NONE', *, *, #5914, .F. ) ;
#13342 = ORIENTED_EDGE ( 'NONE', *, *, #2150, .T. ) ;
#13343 = CARTESIAN_POINT ( 'NONE',  ( 635.0000000000000000, 160.0000000000000284, 187.5000000000000000 ) ) ;
#13344 = FACE_OUTER_BOUND ( 'NONE', #1869, .T. ) ;
#13345 = DIRECTION ( 'NONE',  ( 1.000000000000000000, 0.000000000000000000, 0.000000000000000000 ) ) ;
#13346 = CARTESIAN_POINT ( 'NONE',  ( 635.0000000000000000, 160.0000000000000284, 207.0000000000000000 ) ) ;
#13347 = CARTESIAN_POINT ( 'NONE',  ( 6.725979247667768668, 3.622307570260308918, -6.470294263593358686 ) ) ;
#13348 = DIRECTION ( 'NONE',  ( 0.000000000000000000, 0.000000000000000000, 1.000000000000000000 ) ) ;
#13349 = LINE ( 'NONE', #14316, #7239 ) ;
#13350 = VERTEX_POINT ( 'NONE', #7248 ) ;
#13351 = CARTESIAN_POINT ( 'NONE',  ( 0.000000000000000000, 0.000000000000000000, 0.000000000000000000 ) ) ;
#13352 = CARTESIAN_POINT ( 'NONE',  ( 0.000000000000000000, 0.000000000000000000, 0.000000000000000000 ) ) ;
#13353 = APPLICATION_PROTOCOL_DEFINITION ( 'draft international standard', 'automotive_design', 1998, #13377 ) ;
#13354 = LINE ( 'NONE', #2208, #6150 ) ;
#13355 = ORIENTED_EDGE ( 'NONE', *, *, #6759, .F. ) ;
#13356 = ORIENTED_EDGE ( 'NONE', *, *, #9785, .T. ) ;
#13357 = SURFACE_SIDE_STYLE ('',( #5610 ) ) ;
#13358 = PLANE ( 'NONE',  #6383 ) ;
#13359 = CIRCLE ( 'NONE', #623, 4.799999999999968736 ) ;
#13360 = CARTESIAN_POINT ( 'NONE',  ( 43.50000000000000711, 0.000000000000000000, 0.000000000000000000 ) ) ;
#13361 = DIRECTION ( 'NONE',  ( 1.000000000000000000, 0.000000000000000000, 0.000000000000000000 ) ) ;
#13362 = VERTEX_POINT ( 'NONE', #14050 ) ;
#13363 = DIRECTION ( 'NONE',  ( 1.000000000000000000, 0.000000000000000000, 0.000000000000000000 ) ) ;
#13364 = ORIENTED_EDGE ( 'NONE', *, *, #9374, .F. ) ;
#13365=STYLED_ITEM('',(#14674),#2170);
#13366 = TOROIDAL_SURFACE ( 'NONE', #7946, 6.250000000000000000, 0.7500000000000000000 ) ;
#13367 = DIRECTION ( 'NONE',  ( -1.148424442117026787E-15, 3.445273326351093279E-16, 1.000000000000000000 ) ) ;
#13368 = CARTESIAN_POINT ( 'NONE',  ( 10.00000000000000000, -9.999999999999998224, 190.0000000000000000 ) ) ;
#13369 = SHAPE_REPRESENTATION_RELATIONSHIP ( 'NONE' , 'NONE' ,  #9337, #4067 ) ;
#13370 = PRODUCT_DEFINITION_SHAPE ( 'NONE', 'NONE',  #14645 ) ;
#13371 = ADVANCED_FACE ( 'NONE', ( #5054 ), #5269, .F. ) ;
#13372 = CARTESIAN_POINT ( 'NONE',  ( 642.0000000000000000, 167.0000000000000000, -233.5000000000000000 ) ) ;
#13373 = ADVANCED_FACE ( 'NONE', ( #449 ), #2333, .T. ) ;
#13374 = VERTEX_POINT ( 'NONE', #14374 ) ;
#13375 = ORIENTED_EDGE ( 'NONE', *, *, #5481, .T. ) ;
#13376 = DIRECTION ( 'NONE',  ( 0.000000000000000000, 0.000000000000000000, -1.000000000000000000 ) ) ;
#13377 = APPLICATION_CONTEXT ( 'automotive_design' ) ;
#13378 =( BOUNDED_SURFACE ( )  B_SPLINE_SURFACE ( 3, 2, ( 
 ( #13741, #8115, #12620 ),
 ( #8179, #2580, #7083 ),
 ( #815, #10041, #3256 ),
 ( #2062, #11156, #13444 ),
 ( #4372, #14547, #1101 ),
 ( #5331, #14333, #2144 ) ),
 .UNSPECIFIED., .F., .F., .T. ) 
 B_SPLINE_SURFACE_WITH_KNOTS ( ( 4, 2, 4 ),
 ( 3, 3 ),
 ( 0.003190620565844218184, 0.007281897438794484971, 0.01137317431174475132 ),
 ( 0.000000000000000000, 1.000000000000000000 ),
 .UNSPECIFIED. ) 
 GEOMETRIC_REPRESENTATION_ITEM ( )  RATIONAL_B_SPLINE_SURFACE ( (
 ( 1.000000000000000000, 0.8047731410850399447, 1.000000000000000000),
 ( 1.000000000000000000, 0.8125552299156222347, 1.000000000000000000),
 ( 1.000000000000000000, 0.8191520442889872466, 1.000000000000000000),
 ( 1.000000000000000000, 0.8191520442889872466, 1.000000000000000000),
 ( 1.000000000000000000, 0.8125552299156223457, 1.000000000000000000),
 ( 1.000000000000000000, 0.8047731410850402778, 1.000000000000000000) ) ) 
 REPRESENTATION_ITEM ( '' )  SURFACE ( )  );
#13379 = DIRECTION ( 'NONE',  ( -1.000000000000000000, 0.000000000000000000, 0.000000000000000000 ) ) ;
#13380 = CARTESIAN_POINT ( 'NONE',  ( 446.3084422793565409, 264.0194060144110608, 187.0000000000000000 ) ) ;
#13381 = AXIS2_PLACEMENT_3D ( 'NONE', #1587, #9281, #3957 ) ;
#13382 = ORIENTED_EDGE ( 'NONE', *, *, #7283, .F. ) ;
#13383 = ORIENTED_EDGE ( 'NONE', *, *, #2833, .T. ) ;
#13384 = DIRECTION ( 'NONE',  ( 1.000000000000000000, 0.000000000000000000, -0.000000000000000000 ) ) ;
#13385 = DIRECTION ( 'NONE',  ( 0.000000000000000000, 1.224646799147343593E-16, 1.000000000000000000 ) ) ;
#13386 = CARTESIAN_POINT ( 'NONE',  ( 0.02448733951239481094, 4.877042772274728044, -3.751161874094022242 ) ) ;
#13387 = LINE ( 'NONE', #14503, #1106 ) ;
#13388 = FILL_AREA_STYLE ('',( #12579 ) ) ;
#13389 =( LENGTH_UNIT ( ) NAMED_UNIT ( * ) SI_UNIT ( .MILLI., .METRE. ) );
#13390 = EDGE_CURVE ( 'NONE', #6556, #9876, #848, .T. ) ;
#13391 = ORIENTED_EDGE ( 'NONE', *, *, #8833, .T. ) ;
#13392 = AXIS2_PLACEMENT_3D ( 'NONE', #3021, #9454, #725 ) ;
#13393 = CARTESIAN_POINT ( 'NONE',  ( 0.000000000000000000, 4.330127018922190985, -2.500000000000007105 ) ) ;
#13394 = AXIS2_PLACEMENT_3D ( 'NONE', #13302, #12180, #8943 ) ;
#13395 = VERTEX_POINT ( 'NONE', #2033 ) ;
#13396 = VERTEX_POINT ( 'NONE', #713 ) ;
#13397 = LINE ( 'NONE', #7659, #7574 ) ;
#13398 = ORIENTED_EDGE ( 'NONE', *, *, #14083, .T. ) ;
#13399 = EDGE_CURVE ( 'NONE', #483, #9509, #4270, .T. ) ;
#13400 = CARTESIAN_POINT ( 'NONE',  ( 723.8855453127956707, 217.2873478855657368, -6.736265118569116382E-13 ) ) ;
#13401 = CARTESIAN_POINT ( 'NONE',  ( 0.4465819873851989974, -2.886751345948121106, 4.999999999999999112 ) ) ;
#13402 = AXIS2_PLACEMENT_3D ( 'NONE', #9430, #400, #5421 ) ;
#13403 = AXIS2_PLACEMENT_3D ( 'NONE', #4445, #8944, #7853 ) ;
#13404 = ORIENTED_EDGE ( 'NONE', *, *, #7150, .T. ) ;
#13405 = CARTESIAN_POINT ( 'NONE',  ( 139.8040310085880833, 355.9707293956415697, -187.0000000000000000 ) ) ;
#13406 = CARTESIAN_POINT ( 'NONE',  ( 635.0000000000000000, 160.0000000000000284, -187.5000000000000000 ) ) ;
#13407 = CARTESIAN_POINT ( 'NONE',  ( -2.971071886220377323, -5.790204346174079753, -4.679857033580009373E-15 ) ) ;
#13408 = DIRECTION ( 'NONE',  ( -1.000000000000000000, 0.000000000000000000, 0.000000000000000000 ) ) ;
#13409 = ADVANCED_FACE ( 'NONE', ( #3086, #13192 ), #3009, .T. ) ;
#13410 = VERTEX_POINT ( 'NONE', #6549 ) ;
#13411 = VECTOR ( 'NONE', #7475, 1000.000000000000000 ) ;
#13412 = SURFACE_STYLE_USAGE ( .BOTH. , #7671 ) ;
#13413 = EDGE_LOOP ( 'NONE', ( #14027, #11182, #2058, #8710 ) ) ;
#13414 = VECTOR ( 'NONE', #10849, 1000.000000000000000 ) ;
#13415 = AXIS2_PLACEMENT_3D ( 'NONE', #6404, #4178, #3075 ) ;
#13416 = ORIENTED_EDGE ( 'NONE', *, *, #7715, .T. ) ;
#13417 = DIRECTION ( 'NONE',  ( -1.000000000000000000, 0.000000000000000000, 0.000000000000000000 ) ) ;
#13418 = EDGE_CURVE ( 'NONE', #9996, #2290, #8691, .T. ) ;
#13419 = CARTESIAN_POINT ( 'NONE',  ( -1.891202423064421949E-13, -6.304008076881404142E-13, -189.9999999999986358 ) ) ;
#13420 = CARTESIAN_POINT ( 'NONE',  ( 627.5000000000000000, 160.0000000000000284, -210.0000059999999849 ) ) ;
#13421 = EDGE_CURVE ( 'NONE', #1005, #5487, #4719, .T. ) ;
#13422 = PRODUCT_RELATED_PRODUCT_CATEGORY ( 'part', '', ( #8554 ) ) ;
#13423 = DIRECTION ( 'NONE',  ( 0.000000000000000000, -0.5000000000000009992, 0.8660254037844381525 ) ) ;
#13424 = VECTOR ( 'NONE', #12896, 1000.000000000000000 ) ;
#13425 = CIRCLE ( 'NONE', #8948, 6.750000000000000000 ) ;
#13426 = CARTESIAN_POINT ( 'NONE',  ( 0.2494252716035025574, 1.935831255942362494, -4.000000000000000000 ) ) ;
#13427 = CARTESIAN_POINT ( 'NONE',  ( 144.7991633467111683, 386.6211705227183870, -210.0000000000000000 ) ) ;
#13428 = CARTESIAN_POINT ( 'NONE',  ( 148.9991633467111569, 386.6211705227183870, 210.0000000000000000 ) ) ;
#13429 = ORIENTED_EDGE ( 'NONE', *, *, #6217, .T. ) ;
#13430 = CARTESIAN_POINT ( 'NONE',  ( 455.5035746174796714, 294.6698471414878782, 187.0000000000000568 ) ) ;
#13431 = DIRECTION ( 'NONE',  ( 0.000000000000000000, 0.000000000000000000, -1.000000000000000000 ) ) ;
#13432 = ITEM_DEFINED_TRANSFORMATION ( 'NONE', 'NONE', #5247,  #9440 ) ;
#13433 = CIRCLE ( 'NONE', #468, 2.500000000000000444 ) ;
#13434 = DIRECTION ( 'NONE',  ( -0.8191520442889875797, 1.003171929053519570E-16, 0.5735764363510522656 ) ) ;
#13435 = ORIENTED_EDGE ( 'NONE', *, *, #58, .F. ) ;
#13436 = ORIENTED_EDGE ( 'NONE', *, *, #12824, .F. ) ;
#13437 =( NAMED_UNIT ( * ) SI_UNIT ( $, .STERADIAN. ) SOLID_ANGLE_UNIT ( ) );
#13438 = CARTESIAN_POINT ( 'NONE',  ( 635.0000000000000000, 160.0000000000000284, -211.0000000000000000 ) ) ;
#13439 = CIRCLE ( 'NONE', #7303, 2.500000000000000888 ) ;
#13440 = VECTOR ( 'NONE', #1585, 1000.000000000000000 ) ;
#13441 = CARTESIAN_POINT ( 'NONE',  ( 139.8040310085880833, 355.9707293956415697, -187.0000000000000000 ) ) ;
#13442 = PRODUCT_DEFINITION ( 'UNKNOWN', '', #3845, #3107 ) ;
#13443 = AXIS2_PLACEMENT_3D ( 'NONE', #10719, #588, #958 ) ;
#13444 = CARTESIAN_POINT ( 'NONE',  ( -4.574783636564603739, 5.228990388888020036, -6.171384342982724647 ) ) ;
#13445 = AXIS2_PLACEMENT_3D ( 'NONE', #13515, #7756, #9146 ) ;
#13446 = EDGE_LOOP ( 'NONE', ( #2349, #6825, #9148, #8340, #5922 ) ) ;
#13447 = UNCERTAINTY_MEASURE_WITH_UNIT (LENGTH_MEASURE( 1.000000000000000082E-05 ), #2705, 'distance_accuracy_value', 'NONE');
#13448 = DIRECTION ( 'NONE',  ( -0.000000000000000000, -0.000000000000000000, -1.000000000000000000 ) ) ;
#13449 = ORIENTED_EDGE ( 'NONE', *, *, #14225, .F. ) ;
#13450 = AXIS2_PLACEMENT_3D ( 'NONE', #6973, #4627, #244 ) ;
#13451 = EDGE_CURVE ( 'NONE', #11290, #5571, #4007, .T. ) ;
#13452 = AXIS2_PLACEMENT_3D ( 'NONE', #4580, #12538, #9071 ) ;
#13453 = CARTESIAN_POINT ( 'NONE',  ( 610.0000000000000000, 227.4403065089105951, 210.0000000000000000 ) ) ;
#13454 = CYLINDRICAL_SURFACE ( 'NONE', #7039, 0.7499999999999997780 ) ;
#13455 = ADVANCED_FACE ( 'NONE', ( #12084 ), #9667, .T. ) ;
#13456 = FACE_OUTER_BOUND ( 'NONE', #13204, .T. ) ;
#13457 = EDGE_LOOP ( 'NONE', ( #5848, #8593 ) ) ;
#13458 = ORIENTED_EDGE ( 'NONE', *, *, #8850, .T. ) ;
#13459 = VECTOR ( 'NONE', #14253, 999.9999999999997726 ) ;
#13460 = LINE ( 'NONE', #7858, #731 ) ;
#13461 = AXIS2_PLACEMENT_3D ( 'NONE', #14512, #4401, #7582 ) ;
#13462 = LINE ( 'NONE', #3357, #10583 ) ;
#13463 = CIRCLE ( 'NONE', #12992, 4.000000000000000000 ) ;
#13464 = CARTESIAN_POINT ( 'NONE',  ( 4.000000000001088907, 1.658577278524410170, -3.531553309554541720 ) ) ;
#13465 = ORIENTED_EDGE ( 'NONE', *, *, #7666, .F. ) ;
#13466 = EDGE_CURVE ( 'NONE', #13276, #2544, #4344, .T. ) ;
#13467 = AXIS2_PLACEMENT_3D ( 'NONE', #13119, #5306, #1974 ) ;
#13468 = EDGE_LOOP ( 'NONE', ( #13355, #9089, #4815, #10330 ) ) ;
#13469 = DIRECTION ( 'NONE',  ( 0.000000000000000000, -1.000000000000000000, 0.000000000000000000 ) ) ;
#13470 = CIRCLE ( 'NONE', #7817, 2.199999999999746159 ) ;
#13471 = DIRECTION ( 'NONE',  ( 0.000000000000000000, 0.000000000000000000, 1.000000000000000000 ) ) ;
#13472 = CARTESIAN_POINT ( 'NONE',  ( -1.317756351988340180, 3.857995168970202116, -0.04852650426601388955 ) ) ;
#13473 = PRESENTATION_STYLE_ASSIGNMENT (( #12278 ) ) ;
#13474 = PRODUCT ( 'hex flange bolt small_iso_ISO 4162 - M8 x 35 x 22-N', 'hex flange bolt small_iso_ISO 4162 - M8 x 35 x 22-N', '', ( #737 ) ) ;
#13475 = ORIENTED_EDGE ( 'NONE', *, *, #13418, .T. ) ;
#13476 = MECHANICAL_DESIGN_GEOMETRIC_PRESENTATION_REPRESENTATION (  '', ( #1453 ), #9232 ) ;
#13477 = LINE ( 'NONE', #14, #13678 ) ;
#13478 = ORIENTED_EDGE ( 'NONE', *, *, #4575, .T. ) ;
#13479 = ORIENTED_EDGE ( 'NONE', *, *, #14608, .T. ) ;
#13480 = DIRECTION ( 'NONE',  ( 0.000000000000000000, 0.5000000000000018874, 0.8660254037844375974 ) ) ;
#13481 = ORIENTED_EDGE ( 'NONE', *, *, #7164, .F. ) ;
#13482 = AXIS2_PLACEMENT_3D ( 'NONE', #1739, #7202, #5956 ) ;
#13483 = CARTESIAN_POINT ( 'NONE',  ( 0.000000000000000000, -4.330127018922194537, -2.500000000000000444 ) ) ;
#13484 = EDGE_CURVE ( 'NONE', #12461, #4246, #12212, .T. ) ;
#13485 = FACE_OUTER_BOUND ( 'NONE', #7903, .T. ) ;
#13486 = AXIS2_PLACEMENT_3D ( 'NONE', #8058, #2735, #1554 ) ;
#13487 = ORIENTED_EDGE ( 'NONE', *, *, #3943, .F. ) ;
#13488 = CARTESIAN_POINT ( 'NONE',  ( -1.059638217015129330E-15, 0.4887495715076925484, 4.999999999999999112 ) ) ;
#13489 = CARTESIAN_POINT ( 'NONE',  ( 650.0000000000000000, 175.0000000000000568, 190.0000000000000000 ) ) ;
#13490 = CARTESIAN_POINT ( 'NONE',  ( 5.991014884144048480, 2.818925648462311528E-15, 4.999999999999999112 ) ) ;
#13491 = CARTESIAN_POINT ( 'NONE',  ( 650.0000000000000000, 145.0000000000000568, 210.0000000000000000 ) ) ;
#13492 =( NAMED_UNIT ( * ) PLANE_ANGLE_UNIT ( ) SI_UNIT ( $, .RADIAN. ) );
#13493 = AXIS2_PLACEMENT_3D ( 'NONE', #2430, #1316, #5890 ) ;
#13494 = ORIENTED_EDGE ( 'NONE', *, *, #14432, .T. ) ;
#13495 = CARTESIAN_POINT ( 'NONE',  ( 705.2654023280961155, 165.6605111121464518, 177.6000000000000512 ) ) ;
#13496 = ORIENTED_EDGE ( 'NONE', *, *, #14584, .F. ) ;
#13497 = VECTOR ( 'NONE', #2818, 1000.000000000000000 ) ;
#13498 = ORIENTED_EDGE ( 'NONE', *, *, #14132, .F. ) ;
#13499 = CARTESIAN_POINT ( 'NONE',  ( 112.9652219749295341, 376.5507399164317803, 190.0000000000000000 ) ) ;
#13500 = CARTESIAN_POINT ( 'NONE',  ( 640.0000000000000000, 160.0000000000000284, -222.5000000000000000 ) ) ;
#13501 = VECTOR ( 'NONE', #554, 1000.000000000000227 ) ;
#13502 = ADVANCED_FACE ( 'NONE', ( #6256, #9951 ), #9869, .T. ) ;
#13503 = CARTESIAN_POINT ( 'NONE',  ( 0.000000000000000000, 5.051668046482832750E-16, -4.000000000000000000 ) ) ;
#13504 = FACE_OUTER_BOUND ( 'NONE', #13197, .T. ) ;
#13505 = EDGE_CURVE ( 'NONE', #13769, #11016, #5183, .T. ) ;
#13506 = APPLICATION_PROTOCOL_DEFINITION ( 'draft international standard', 'automotive_design', 1998, #6777 ) ;
#13507 = DIRECTION ( 'NONE',  ( 0.5000000000000006661, 0.8660254037844383745, -0.000000000000000000 ) ) ;
#13508 = LINE ( 'NONE', #12609, #12491 ) ;
#13509 = PLANE ( 'NONE',  #3652 ) ;
#13510 = VERTEX_POINT ( 'NONE', #13059 ) ;
#13511 = ADVANCED_FACE ( 'NONE', ( #7437 ), #5417, .T. ) ;
#13512 = CARTESIAN_POINT ( 'NONE',  ( -2.241046694638765935, -6.576374040526340892, -6.171384342982618065 ) ) ;
#13513 = CARTESIAN_POINT ( 'NONE',  ( 6.533910050139697390, -5.901028503456124952, 6.252275320486994560E-15 ) ) ;
#13514 = CONTEXT_DEPENDENT_SHAPE_REPRESENTATION ( #8295, #372 ) ;
#13517 = EDGE_CURVE ( 'NONE', #7485, #12397, #11922, .T. ) ;
#13516 = AXIS2_PLACEMENT_3D ( 'NONE', #8358, #7182, #10792 ) ;
#13515 = CARTESIAN_POINT ( 'NONE',  ( 635.0000000000000000, 160.0000000000000284, 187.5000000000000000 ) ) ;
#13518 = ORIENTED_EDGE ( 'NONE', *, *, #10355, .F. ) ;
#13519 = ORIENTED_EDGE ( 'NONE', *, *, #7454, .F. ) ;
#13520 = DIRECTION ( 'NONE',  ( -1.000000000000000000, 0.000000000000000000, 0.000000000000000000 ) ) ;
#13521 = CARTESIAN_POINT ( 'NONE',  ( 455.5035746174796714, 294.6698471414878782, 210.0000000000000000 ) ) ;
#13522 = DIRECTION ( 'NONE',  ( -1.000000000000000000, -0.000000000000000000, -0.000000000000000000 ) ) ;
#13523 = CARTESIAN_POINT ( 'NONE',  ( 3.978477517404916064, 5.573260695678954768, -6.171287963165197787 ) ) ;
#13524 = DIRECTION ( 'NONE',  ( 0.000000000000000000, 0.000000000000000000, -1.000000000000000000 ) ) ;
#13525 = ORIENTED_EDGE ( 'NONE', *, *, #7288, .T. ) ;
#13526 = EDGE_CURVE ( 'NONE', #2452, #12673, #10833, .T. ) ;
#13527 = EDGE_CURVE ( 'NONE', #13261, #3214, #6594, .T. ) ;
#13528 = FACE_OUTER_BOUND ( 'NONE', #3733, .T. ) ;
#13529 = LINE ( 'NONE', #3416, #7027 ) ;
#13530 = FILL_AREA_STYLE_COLOUR ( '', #1934 ) ;
#13531 = FACE_BOUND ( 'NONE', #309, .T. ) ;
#13532 = ORIENTED_EDGE ( 'NONE', *, *, #547, .F. ) ;
#13533 = ORIENTED_EDGE ( 'NONE', *, *, #6792, .T. ) ;
#13534 = CARTESIAN_POINT ( 'NONE',  ( -8.505790995054894665, 376.6597771564184427, 184.8000000000000398 ) ) ;
#13535 = LINE ( 'NONE', #981, #14586 ) ;
#13536 = EDGE_CURVE ( 'NONE', #10228, #10517, #1156, .T. ) ;
#13537 = CARTESIAN_POINT ( 'NONE',  ( -4.197393957002303999, -7.773935952363655451E-14, -3.503767560748929810 ) ) ;
#13538 = ORIENTED_EDGE ( 'NONE', *, *, #4868, .F. ) ;
#13539 = ORIENTED_EDGE ( 'NONE', *, *, #12553, .T. ) ;
#13540 = CARTESIAN_POINT ( 'NONE',  ( 609.7898554267394502, 185.8834251265051307, -186.1610889986683048 ) ) ;
#13541 = CARTESIAN_POINT ( 'NONE',  ( 636.7717819724297215, 155.3244477714206653, 215.5000000000000000 ) ) ;
#13542 = FACE_OUTER_BOUND ( 'NONE', #11561, .T. ) ;
#13543 = CARTESIAN_POINT ( 'NONE',  ( 1.734723475976807094E-15, 4.618802153517012954, -0.4999999999999995559 ) ) ;
#13544 = CYLINDRICAL_SURFACE ( 'NONE', #11618, 5.000000000000004441 ) ;
#13545 = VERTEX_POINT ( 'NONE', #9200 ) ;
#13546 = DIRECTION ( 'NONE',  ( 1.000000000000000000, 0.000000000000000000, 0.000000000000000000 ) ) ;
#13547 = VERTEX_POINT ( 'NONE', #8015 ) ;
#13548 = VERTEX_POINT ( 'NONE', #13708 ) ;
#13549 = FACE_OUTER_BOUND ( 'NONE', #4297, .T. ) ;
#13550 = ORIENTED_EDGE ( 'NONE', *, *, #4590, .F. ) ;
#13551 = CARTESIAN_POINT ( 'NONE',  ( -8.505790995054940851, 376.6597771564182722, -190.0000000000000284 ) ) ;
#13552 = DIRECTION ( 'NONE',  ( 0.000000000000000000, 0.000000000000000000, 1.000000000000000000 ) ) ;
#13553 = ORIENTED_EDGE ( 'NONE', *, *, #12846, .F. ) ;
#13554 = FACE_OUTER_BOUND ( 'NONE', #14578, .T. ) ;
#13555 = CARTESIAN_POINT ( 'NONE',  ( 708.1388811837592812, 164.7984674554467404, -177.6000000000002217 ) ) ;
#13556 = CARTESIAN_POINT ( 'NONE',  ( 6.367873360227555679, -2.886751345948120662, 4.999999999999999112 ) ) ;
#13557 = CARTESIAN_POINT ( 'NONE',  ( 1.317756351988342622, -3.857995168970215438, -0.04852650426602527628 ) ) ;
#13558 = ORIENTED_EDGE ( 'NONE', *, *, #1515, .F. ) ;
#13559 = DIRECTION ( 'NONE',  ( 1.000000000000000000, -3.469446951953611033E-15, 0.000000000000000000 ) ) ;
#13560 = ORIENTED_EDGE ( 'NONE', *, *, #10230, .F. ) ;
#13561 = EDGE_CURVE ( 'NONE', #13629, #7886, #2099, .T. ) ;
#13562 = ORIENTED_EDGE ( 'NONE', *, *, #2232, .F. ) ;
#13563 = CARTESIAN_POINT ( 'NONE',  ( 708.1388811837593948, 164.7984674554474225, 177.6000000000001648 ) ) ;
#13564 = CARTESIAN_POINT ( 'NONE',  ( 2.500000000000000000, 1.768423874527822459, -1.021000000000002794 ) ) ;
#13565 = CARTESIAN_POINT ( 'NONE',  ( 0.3461262719736147297, -4.658553426539303821, -3.671615880910379381 ) ) ;
#13566 = CARTESIAN_POINT ( 'NONE',  ( 470.8287951810180516, 310.9528939902474463, 210.0000000000000000 ) ) ;
#13567 = CARTESIAN_POINT ( 'NONE',  ( 0.2484800633749957022, -4.430380094434235971, -0.3263565795980920559 ) ) ;
#13568 = CARTESIAN_POINT ( 'NONE',  ( -6.818286579240217193, 1.325012739682870810, -6.208253321455267759 ) ) ;
#13569 = DIRECTION ( 'NONE',  ( 0.5000000000000005551, -0.8660254037844383745, 0.000000000000000000 ) ) ;
#13570 = APPLICATION_CONTEXT ( 'automotive_design' ) ;
#13571 = ORIENTED_EDGE ( 'NONE', *, *, #3766, .T. ) ;
#13572 = CARTESIAN_POINT ( 'NONE',  ( 0.000000000000000000, 0.000000000000000000, -5.000000000000000000 ) ) ;
#13573 = DIRECTION ( 'NONE',  ( 0.000000000000000000, 0.000000000000000000, 1.000000000000000000 ) ) ;
#13574 = CARTESIAN_POINT ( 'NONE',  ( 6.452281807715713136, -5.797857616946124892, 1.707831949354040044E-16 ) ) ;
#13575 = APPLICATION_PROTOCOL_DEFINITION ( 'draft international standard', 'automotive_design', 1998, #4340 ) ;
#13576 = EDGE_LOOP ( 'NONE', ( #6821, #10170, #11291, #7708 ) ) ;
#13577 = EDGE_CURVE ( 'NONE', #8790, #3368, #5659, .T. ) ;
#13578 = CARTESIAN_POINT ( 'NONE',  ( -6.500000000000000000, -3.752776749732572803, -6.064240316920399998 ) ) ;
#13579 = ORIENTED_EDGE ( 'NONE', *, *, #2401, .T. ) ;
#13580 = ORIENTED_EDGE ( 'NONE', *, *, #1582, .F. ) ;
#13581 = FACE_OUTER_BOUND ( 'NONE', #10907, .T. ) ;
#13582 = CARTESIAN_POINT ( 'NONE',  ( -5.416666666666670515, 4.378239541354659536, -5.848636054922036642 ) ) ;
#13583 = ADVANCED_FACE ( 'NONE', ( #2411 ), #12434, .F. ) ;
#13584 = CARTESIAN_POINT ( 'NONE',  ( 610.0000000000000000, 0.000000000000000000, 210.0000000000000000 ) ) ;
#13585 = ADVANCED_FACE ( 'NONE', ( #5581 ), #6628, .F. ) ;
#13586 = LINE ( 'NONE', #283, #489 ) ;
#13587 = EDGE_CURVE ( 'NONE', #11591, #11781, #12712, .T. ) ;
#13588 = CARTESIAN_POINT ( 'NONE',  ( 6.541171661047876285, -2.934678558896549383, -5.142480235691125223 ) ) ;
#13589 = ORIENTED_EDGE ( 'NONE', *, *, #9828, .F. ) ;
#13590 = CARTESIAN_POINT ( 'NONE',  ( -3.999999999999999112, 1.539600717838996324, -3.300726591567078039 ) ) ;
#13591 = DIRECTION ( 'NONE',  ( -0.9578262852211513190, 0.2873478855663453846, -0.000000000000000000 ) ) ;
#13592 = SURFACE_STYLE_FILL_AREA ( #10273 ) ;
#13593 = CARTESIAN_POINT ( 'NONE',  ( 708.1388811837596222, 164.7984674554460014, -177.6000000000005343 ) ) ;
#13594 = EDGE_LOOP ( 'NONE', ( #12185, #4167, #11463, #7969 ) ) ;
#13595 = ORIENTED_EDGE ( 'NONE', *, *, #7465, .T. ) ;
#13596 = CARTESIAN_POINT ( 'NONE',  ( 703.1581845006096501, 166.2926764603917036, 177.6000000000001648 ) ) ;
#13597 = DIRECTION ( 'NONE',  ( 0.000000000000000000, 0.000000000000000000, -1.000000000000000000 ) ) ;
#13598 = EDGE_CURVE ( 'NONE', #5688, #8553, #13425, .T. ) ;
#13599 = PLANE ( 'NONE',  #10862 ) ;
#13601 = EDGE_LOOP ( 'NONE', ( #6167, #13435, #4954, #10304, #3519, #2156, #9670 ) ) ;
#13600 = CIRCLE ( 'NONE', #13636, 2.199999999999757705 ) ;
#13602 = EDGE_CURVE ( 'NONE', #4648, #4012, #1867, .T. ) ;
#13603 = VECTOR ( 'NONE', #1227, 1000.000000000000114 ) ;
#13604 = CARTESIAN_POINT ( 'NONE',  ( 112.9652219749295341, 376.5507399164317803, -190.0000000000000000 ) ) ;
#13605 = PLANE ( 'NONE',  #11585 ) ;
#13606 = LINE ( 'NONE', #14569, #9194 ) ;
#13607 = DIRECTION ( 'NONE',  ( -1.000000000000000000, 0.000000000000000000, 0.000000000000000000 ) ) ;
#13608 = DIRECTION ( 'NONE',  ( 1.000000000000000000, 0.000000000000000000, 0.000000000000000000 ) ) ;
#13609 = DIRECTION ( 'NONE',  ( -0.000000000000000000, -0.000000000000000000, 1.000000000000000000 ) ) ;
#13610 = SURFACE_STYLE_FILL_AREA ( #4620 ) ;
#13611 = ORIENTED_EDGE ( 'NONE', *, *, #1760, .F. ) ;
#13612 = CARTESIAN_POINT ( 'NONE',  ( 610.0000000000000000, 227.4403065089105951, 190.0000000000000000 ) ) ;
#13613 = ORIENTED_EDGE ( 'NONE', *, *, #12311, .F. ) ;
#13614 = VERTEX_POINT ( 'NONE', #7941 ) ;
#13615 = CARTESIAN_POINT ( 'NONE',  ( 631.0000000000000000, 164.0000000000000284, -233.5000000000000000 ) ) ;
#13616 = VECTOR ( 'NONE', #12317, 1000.000000000000114 ) ;
#13617 = ORIENTED_EDGE ( 'NONE', *, *, #11410, .F. ) ;
#13618 = CONICAL_SURFACE ( 'NONE', #10314, 2.059999999999998721, 0.9599310885968738161 ) ;
#13619 = FACE_OUTER_BOUND ( 'NONE', #12778, .T. ) ;
#13620 = CARTESIAN_POINT ( 'NONE',  ( 153.1991633467111456, 386.6211705227183870, 190.0000000000000000 ) ) ;
#13621 = ORIENTED_EDGE ( 'NONE', *, *, #5499, .T. ) ;
#13622 = CARTESIAN_POINT ( 'NONE',  ( 0.04320752586819773255, 0.9836842030436150353, 4.999999999999999112 ) ) ;
#13623 = DIRECTION ( 'NONE',  ( -0.9578262852211525402, 0.2873478855663419429, 0.000000000000000000 ) ) ;
#13624 = AXIS2_PLACEMENT_3D ( 'NONE', #3726, #78, #13607 ) ;
#13625 = CARTESIAN_POINT ( 'NONE',  ( -4.203833317240879275, -1.627343821129593859, -3.597273115243890818 ) ) ;
#13626 = DIRECTION ( 'NONE',  ( 0.5000000000000022204, 0.8660254037844374864, -0.000000000000000000 ) ) ;
#13627 = ORIENTED_EDGE ( 'NONE', *, *, #12406, .T. ) ;
#13628 = LINE ( 'NONE', #12596, #3534 ) ;
#13629 = VERTEX_POINT ( 'NONE', #10299 ) ;
#13630 = EDGE_CURVE ( 'NONE', #12153, #4733, #14601, .T. ) ;
#13631 = ORIENTED_EDGE ( 'NONE', *, *, #6554, .T. ) ;
#13632 = DIRECTION ( 'NONE',  ( 0.9578262852211513190, -0.2873478855663454401, -1.972152263052529514E-31 ) ) ;
#13633 = AXIS2_PLACEMENT_3D ( 'NONE', #3233, #1014, #858 ) ;
#13634 = VECTOR ( 'NONE', #64, 1000.000000000000000 ) ;
#13636 = AXIS2_PLACEMENT_3D ( 'NONE', #8190, #13972, #11725 ) ;
#13635 = CARTESIAN_POINT ( 'NONE',  ( 635.0000000000000000, 160.0000000000000284, -222.5000000000000000 ) ) ;
#13637 = DIRECTION ( 'NONE',  ( 1.000000000000000000, 0.000000000000000000, 0.000000000000000000 ) ) ;
#13638 = FACE_OUTER_BOUND ( 'NONE', #14581, .T. ) ;
#13639 = CIRCLE ( 'NONE', #10825, 4.000000000000000000 ) ;
#13640 = EDGE_CURVE ( 'NONE', #10478, #173, #4631, .T. ) ;
#13641 = DIRECTION ( 'NONE',  ( -0.2873478855663437193, -0.9578262852211517631, 0.000000000000000000 ) ) ;
#13642 = FACE_OUTER_BOUND ( 'NONE', #7431, .T. ) ;
#13643 = LINE ( 'NONE', #3541, #14565 ) ;
#13644 = EDGE_LOOP ( 'NONE', ( #3097, #6492, #4338, #13834 ) ) ;
#13645 = CIRCLE ( 'NONE', #4934, 3.999999999999999112 ) ;
#13646 = CIRCLE ( 'NONE', #189, 5.000000000000000000 ) ;
#13647 = DIRECTION ( 'NONE',  ( -1.000000000000000000, -0.000000000000000000, -0.000000000000000000 ) ) ;
#13648 = CYLINDRICAL_SURFACE ( 'NONE', #631, 4.799999999999999822 ) ;
#13649 = CARTESIAN_POINT ( 'NONE',  ( 610.7992194312785159, 188.5714065965581483, 184.9452975700425554 ) ) ;
#13650 = ORIENTED_EDGE ( 'NONE', *, *, #622, .T. ) ;
#13651 = DIRECTION ( 'NONE',  ( 0.000000000000000000, 0.000000000000000000, -1.000000000000000000 ) ) ;
#13652 = ORIENTED_EDGE ( 'NONE', *, *, #7541, .F. ) ;
#13653 = ORIENTED_EDGE ( 'NONE', *, *, #12627, .T. ) ;
#13654 = CARTESIAN_POINT ( 'NONE',  ( 4.154306624730763176, -2.398490048084970461, -3.721999068284303824 ) ) ;
#13655 = LINE ( 'NONE', #1178, #1423 ) ;
#13656 = CIRCLE ( 'NONE', #5408, 2.700000000000000178 ) ;
#13657 = CARTESIAN_POINT ( 'NONE',  ( 3.349226789952652439, 2.685125164760731487, -0.2236248678334773199 ) ) ;
#13658 = VECTOR ( 'NONE', #12034, 1000.000000000000000 ) ;
#13659 = CONICAL_SURFACE ( 'NONE', #9180, 5.000000000000000888, 1.047197551196600296 ) ;
#13660 = APPLICATION_CONTEXT ( 'automotive_design' ) ;
#13661 = EDGE_CURVE ( 'NONE', #6556, #5961, #9120, .T. ) ;
#13662 = DIRECTION ( 'NONE',  ( 0.9578262852211513190, -0.2873478855663454401, 2.126837879698859960E-31 ) ) ;
#13663 = LINE ( 'NONE', #3346, #13150 ) ;
#13664 = ORIENTED_EDGE ( 'NONE', *, *, #3437, .T. ) ;
#13665 = VECTOR ( 'NONE', #10069, 1000.000000000000114 ) ;
#13666 = CARTESIAN_POINT ( 'NONE',  ( 237.7887055630606028, 337.0156335382089310, -182.8000000000007219 ) ) ;
#13667 = DIRECTION ( 'NONE',  ( -0.000000000000000000, -0.000000000000000000, -1.000000000000000000 ) ) ;
#13668 = CARTESIAN_POINT ( 'NONE',  ( 635.0000000000000000, 160.0000000000000284, -233.5000000000000284 ) ) ;
#13669 = VECTOR ( 'NONE', #492, 1000.000000000000000 ) ;
#13670 = DIRECTION ( 'NONE',  ( -0.000000000000000000, -0.000000000000000000, -1.000000000000000000 ) ) ;
#13671 = VECTOR ( 'NONE', #4546, 1000.000000000000000 ) ;
#13672 = ORIENTED_EDGE ( 'NONE', *, *, #4228, .T. ) ;
#13673 = ORIENTED_EDGE ( 'NONE', *, *, #6621, .F. ) ;
#13674 = CARTESIAN_POINT ( 'NONE',  ( 4.000000000000000888, 1.539600717838996990, -3.300726591567079815 ) ) ;
#13675 = CARTESIAN_POINT ( 'NONE',  ( 0.000000000000000000, 0.000000000000000000, -1.000000000000000000 ) ) ;
#13676 = CARTESIAN_POINT ( 'NONE',  ( 590.0000000000000000, -9.999999999999941380, -210.0020000000000095 ) ) ;
#13677 = CIRCLE ( 'NONE', #466, 2.649999999999985700 ) ;
#13678 = VECTOR ( 'NONE', #6823, 1000.000000000000000 ) ;
#13679 = DIRECTION ( 'NONE',  ( 0.000000000000000000, 0.000000000000000000, -1.000000000000000000 ) ) ;
#13680 = ADVANCED_FACE ( 'NONE', ( #10163, #6699, #7808 ), #8088, .T. ) ;
#13681 = VECTOR ( 'NONE', #6830, 1000.000000000000000 ) ;
#13682 = ORIENTED_EDGE ( 'NONE', *, *, #7166, .F. ) ;
#13683 = VECTOR ( 'NONE', #6034, 999.9999999999998863 ) ;
#13684 = ORIENTED_EDGE ( 'NONE', *, *, #9994, .F. ) ;
#13685 = CARTESIAN_POINT ( 'NONE',  ( 610.0417734222098716, 190.7948035559919333, -187.0000000000000284 ) ) ;
#13686 = FACE_OUTER_BOUND ( 'NONE', #11161, .T. ) ;
#13687 = LINE ( 'NONE', #6965, #1831 ) ;
#13688 = FACE_BOUND ( 'NONE', #6524, .T. ) ;
#13689 = CYLINDRICAL_SURFACE ( 'NONE', #12810, 4.199999999999981526 ) ;
#13690 = CIRCLE ( 'NONE', #9458, 5.000000000000000888 ) ;
#13691 = EDGE_CURVE ( 'NONE', #6877, #10838, #4566, .T. ) ;
#13692 = ORIENTED_EDGE ( 'NONE', *, *, #12791, .T. ) ;
#13693 = AXIS2_PLACEMENT_3D ( 'NONE', #656, #8574, #5108 ) ;
#13694 = EDGE_CURVE ( 'NONE', #5236, #11071, #11126, .T. ) ;
#13695 = CARTESIAN_POINT ( 'NONE',  ( -3.399999999999999911, 4.163799117101000559E-16, -7.554475477074173106 ) ) ;
#13696 = ORIENTED_EDGE ( 'NONE', *, *, #13154, .T. ) ;
#13697 = ORIENTED_EDGE ( 'NONE', *, *, #1667, .F. ) ;
#13698 = CARTESIAN_POINT ( 'NONE',  ( 6.245813541929282842, 1.036329910263561471, -5.105320956836709279 ) ) ;
#13699 = AXIS2_PLACEMENT_3D ( 'NONE', #1049, #3273, #1953 ) ;
#13700 = EDGE_CURVE ( 'NONE', #7367, #14073, #7881, .T. ) ;
#13701 =( GEOMETRIC_REPRESENTATION_CONTEXT ( 3 ) GLOBAL_UNCERTAINTY_ASSIGNED_CONTEXT ( ( #3704 ) ) GLOBAL_UNIT_ASSIGNED_CONTEXT ( ( #3524, #1370, #5801 ) ) REPRESENTATION_CONTEXT ( 'NONE', 'WORKASPACE' ) );
#13702 = CARTESIAN_POINT ( 'NONE',  ( -8.505790995055050985, 376.6597771564184995, -184.8000000000000398 ) ) ;
#13703 = VECTOR ( 'NONE', #9950, 1000.000000000000114 ) ;
#13704 = VECTOR ( 'NONE', #13328, 1000.000000000000000 ) ;
#13705 = CARTESIAN_POINT ( 'NONE',  ( 639.0000000000000000, 164.0000000000000000, -233.5000000000000000 ) ) ;
#13706 = ORIENTED_EDGE ( 'NONE', *, *, #10896, .F. ) ;
#13707 = CARTESIAN_POINT ( 'NONE',  ( 650.0000000000000000, 0.000000000000000000, 0.000000000000000000 ) ) ;
#13708 = CARTESIAN_POINT ( 'NONE',  ( 6.534838248920899595, -2.951765777552421532, -5.112608298763837489 ) ) ;
#13709 = CIRCLE ( 'NONE', #13943, 2.649999999999985700 ) ;
#13710 = COLOUR_RGB ( '',0.8941176470588234615, 0.8941176470588234615, 0.8941176470588234615 ) ;
#13711 = CYLINDRICAL_SURFACE ( 'NONE', #1348, 0.7500000000000000000 ) ;
#13712 = CARTESIAN_POINT ( 'NONE',  ( 604.3113219698370813, -181.2933965909541598, 182.8000000000001535 ) ) ;
#13713 = ORIENTED_EDGE ( 'NONE', *, *, #7513, .T. ) ;
#13714 = EDGE_CURVE ( 'NONE', #4450, #3047, #447, .T. ) ;
#13715 = LINE ( 'NONE', #10306, #10121 ) ;
#13716 = ORIENTED_EDGE ( 'NONE', *, *, #8065, .F. ) ;
#13717 = CIRCLE ( 'NONE', #2403, 5.000000000000004441 ) ;
#13718 = VERTEX_POINT ( 'NONE', #9056 ) ;
#13719 = DIRECTION ( 'NONE',  ( -0.000000000000000000, -0.000000000000000000, -1.000000000000000000 ) ) ;
#13720 = COLOUR_RGB ( '',1.000000000000000000, 0.9490196078431372140, 0.9098039215686274384 ) ;
#13721 = DIRECTION ( 'NONE',  ( -0.000000000000000000, 1.000000000000000000, -0.000000000000000000 ) ) ;
#13722 = LINE ( 'NONE', #12828, #7809 ) ;
#13723 = EDGE_CURVE ( 'NONE', #14148, #14518, #10593, .T. ) ;
#13724 = CIRCLE ( 'NONE', #5477, 0.5999999999999980904 ) ;
#13725 = ORIENTED_EDGE ( 'NONE', *, *, #4345, .F. ) ;
#13726 = DIRECTION ( 'NONE',  ( 0.9914448613738102711, -0.1305261922200524338, 0.000000000000000000 ) ) ;
#13727 = ADVANCED_FACE ( 'NONE', ( #166 ), #14070, .F. ) ;
#13728 = CARTESIAN_POINT ( 'NONE',  ( 153.1991633467111456, 386.6211705227183870, -210.0000000000000000 ) ) ;
#13729 = CARTESIAN_POINT ( 'NONE',  ( 708.1388811837593948, 164.7984674554466551, -182.7999999999999545 ) ) ;
#13730 = CARTESIAN_POINT ( 'NONE',  ( -1.269541193505925744E-15, 7.895640089090863789, -6.564402953523717166 ) ) ;
#13731 = ORIENTED_EDGE ( 'NONE', *, *, #9551, .T. ) ;
#13732 = CARTESIAN_POINT ( 'NONE',  ( 6.495567275914607031, -5.834887664330119961, -8.422077706216564275E-17 ) ) ;
#13733 = DIRECTION ( 'NONE',  ( 1.000000000000000000, 0.000000000000000000, 0.000000000000000000 ) ) ;
#13734 = DIRECTION ( 'NONE',  ( 0.000000000000000000, 1.000000000000000000, 0.000000000000000000 ) ) ;
#13735 = CARTESIAN_POINT ( 'NONE',  ( -5.357619327558936585E-16, 7.505553499465137612, -6.064240316920400886 ) ) ;
#13736 = ORIENTED_EDGE ( 'NONE', *, *, #6407, .T. ) ;
#13737 = CARTESIAN_POINT ( 'NONE',  ( 6.245835795331710294, -1.036512332922514767, 5.105321605219339531 ) ) ;
#13738 = EDGE_LOOP ( 'NONE', ( #1399, #867, #12235, #11015, #1112, #7931, #4761, #9177, #3934, #14372, #2935, #8204 ) ) ;
#13739 = ORIENTED_EDGE ( 'NONE', *, *, #10626, .T. ) ;
#13740 = AXIS2_PLACEMENT_3D ( 'NONE', #6416, #716, #13408 ) ;
#13741 = CARTESIAN_POINT ( 'NONE',  ( 0.2813450144774485850, 7.667988119308852824, -6.122077150241853616 ) ) ;
#13742 = DIRECTION ( 'NONE',  ( -1.000000000000000000, -6.938893903907222067E-15, 0.000000000000000000 ) ) ;
#13743 = CARTESIAN_POINT ( 'NONE',  ( 112.9652219749295341, 376.5507399164317803, -210.0000000000000000 ) ) ;
#13744 = PRODUCT_DEFINITION_CONTEXT ( 'detailed design', #2246, 'design' ) ;
#13745 = VECTOR ( 'NONE', #5854, 1000.000000000000000 ) ;
#13746 = CARTESIAN_POINT ( 'NONE',  ( 6.500000000000000000, 3.752776749732563921, -8.000000000000000000 ) ) ;
#13747 = ORIENTED_EDGE ( 'NONE', *, *, #6914, .F. ) ;
#13748 = DIRECTION ( 'NONE',  ( 0.2873478855663417764, 0.9578262852211525402, 0.000000000000000000 ) ) ;
#13749 = DIRECTION ( 'NONE',  ( 1.000000000000000000, 0.000000000000000000, -0.000000000000000000 ) ) ;
#13750 = CARTESIAN_POINT ( 'NONE',  ( 0.000000000000000000, 0.000000000000000000, 0.000000000000000000 ) ) ;
#13751 = LINE ( 'NONE', #3644, #12253 ) ;
#13752 = VERTEX_POINT ( 'NONE', #3956 ) ;
#13753 = ORIENTED_EDGE ( 'NONE', *, *, #25, .T. ) ;
#13754 = DIRECTION ( 'NONE',  ( -0.000000000000000000, -0.000000000000000000, -1.000000000000000000 ) ) ;
#13755 = CARTESIAN_POINT ( 'NONE',  ( 4.211140560182196957, -2.431303136016555122, -3.745885042887436622 ) ) ;
#13756 = ADVANCED_FACE ( 'NONE', ( #5957 ), #11472, .F. ) ;
#13757 = CARTESIAN_POINT ( 'NONE',  ( -3.098410542199071749, -7.060458129626440815, -1.000000000000000000 ) ) ;
#13758 = CLOSED_SHELL ( 'NONE', ( #7378, #3585, #3129, #6284, #87, #8750, #11022, #1782, #13196, #11775, #11254, #8339, #4533, #12401, #590, #9498, #5061, #2729, #6060, #10948, #2584 ) ) ;
#13759 = ORIENTED_EDGE ( 'NONE', *, *, #9050, .T. ) ;
#13760 = ORIENTED_EDGE ( 'NONE', *, *, #2127, .F. ) ;
#13761 = CARTESIAN_POINT ( 'NONE',  ( 610.8620436566991430, 188.5525593289319488, -184.8000000000000682 ) ) ;
#13762 = CARTESIAN_POINT ( 'NONE',  ( 2.500000000000000000, -1.768423874527823569, 1.021000000000002350 ) ) ;
#13763 = DIRECTION ( 'NONE',  ( 0.2873478855663452736, 0.9578262852211513190, 3.491481338843133355E-15 ) ) ;
#13764 = CYLINDRICAL_SURFACE ( 'NONE', #8903, 5.199999999999999289 ) ;
#13765 = CARTESIAN_POINT ( 'NONE',  ( -4.555432764205793461, 5.242992371775927474, -6.208169345099788572 ) ) ;
#13766 = ORIENTED_EDGE ( 'NONE', *, *, #13390, .F. ) ;
#13767 = CARTESIAN_POINT ( 'NONE',  ( 4.141042297810615835, -2.227970268150433863, -3.687027686973623819 ) ) ;
#13768 = ORIENTED_EDGE ( 'NONE', *, *, #10260, .F. ) ;
#13769 = VERTEX_POINT ( 'NONE', #12591 ) ;
#13770 = PLANE ( 'NONE',  #13229 ) ;
#13771 = ADVANCED_FACE ( 'NONE', ( #2475 ), #5007, .F. ) ;
#13772 = ADVANCED_FACE ( 'NONE', ( #7203 ), #6978, .F. ) ;
#13773 = PLANE ( 'NONE',  #13450 ) ;
#13774 =( REPRESENTATION_RELATIONSHIP ('NONE','NONE', #2822, #9337 ) REPRESENTATION_RELATIONSHIP_WITH_TRANSFORMATION ( #10823 )SHAPE_REPRESENTATION_RELATIONSHIP( ) );
#13775 = DIRECTION ( 'NONE',  ( 0.000000000000000000, 0.000000000000000000, -1.000000000000000000 ) ) ;
#13776 = ADVANCED_FACE ( 'NONE', ( #6178 ), #8308, .T. ) ;
#13777 = B_SPLINE_CURVE_WITH_KNOTS ( 'NONE', 3,
 ( #2135, #3468, #7902, #2273, #6785, #7836 ),
 .UNSPECIFIED., .F., .F.,
 ( 4, 2, 4 ),
 ( 0.000000000000000000, 0.0003352299596267567321, 0.0006704599192535134642 ),
 .UNSPECIFIED. ) ;
#13778 = EDGE_LOOP ( 'NONE', ( #14423, #4875 ) ) ;
#13779 = CARTESIAN_POINT ( 'NONE',  ( 113.8272656316285776, 379.4242187720952870, 1.650218294979717018E-14 ) ) ;
#13780 = PLANE ( 'NONE',  #7304 ) ;
#13781 = EDGE_CURVE ( 'NONE', #6858, #7308, #11691, .T. ) ;
#13782 = PLANE ( 'NONE',  #5835 ) ;
#13783 = CARTESIAN_POINT ( 'NONE',  ( 1.734723475976807094E-15, 4.618802153517012954, -0.4999999999999995559 ) ) ;
#13784 = ORIENTED_EDGE ( 'NONE', *, *, #5830, .T. ) ;
#13785 = CARTESIAN_POINT ( 'NONE',  ( 0.000000000000000000, 0.000000000000000000, -5.000000000000000000 ) ) ;
#13786 = EDGE_LOOP ( 'NONE', ( #2182, #12415, #11299, #6939, #10130 ) ) ;
#13787 = ORIENTED_EDGE ( 'NONE', *, *, #13527, .F. ) ;
#13788 = LINE ( 'NONE', #328, #5615 ) ;
#13789 = DIRECTION ( 'NONE',  ( -0.2873478855663453846, -0.9578262852211513190, -0.000000000000000000 ) ) ;
#13790 = EDGE_CURVE ( 'NONE', #14129, #1376, #7049, .T. ) ;
#13791 = CARTESIAN_POINT ( 'NONE',  ( 636.9746078850427011, 155.6249658629529620, -210.0000000000000000 ) ) ;
#13792 = EDGE_CURVE ( 'NONE', #2766, #3675, #705, .T. ) ;
#13793 = EDGE_LOOP ( 'NONE', ( #7157, #5584, #14426, #620 ) ) ;
#13794 = CARTESIAN_POINT ( 'NONE',  ( 5.560781378645575757, 0.000000000000000000, -4.000000000000000000 ) ) ;
#13795 = ADVANCED_FACE ( 'NONE', ( #9570 ), #13780, .F. ) ;
#13796 = DIRECTION ( 'NONE',  ( -0.000000000000000000, -0.000000000000000000, 1.000000000000000000 ) ) ;
#13797 = CARTESIAN_POINT ( 'NONE',  ( 43.50000000000000711, 4.052968581778165278E-16, -3.309499999999999886 ) ) ;
#13798 = CARTESIAN_POINT ( 'NONE',  ( -0.02511973781850462134, 4.877415612947412882, -3.751298745799839462 ) ) ;
#13799 = ORIENTED_EDGE ( 'NONE', *, *, #7077, .T. ) ;
#13800 = DIRECTION ( 'NONE',  ( -0.000000000000000000, -0.000000000000000000, 1.000000000000000000 ) ) ;
#13801 =( NAMED_UNIT ( * ) PLANE_ANGLE_UNIT ( ) SI_UNIT ( $, .RADIAN. ) );
#13802 = ITEM_DEFINED_TRANSFORMATION ( 'NONE', 'NONE', #11603,  #9440 ) ;
#13803 = ORIENTED_EDGE ( 'NONE', *, *, #10451, .F. ) ;
#13804 = CARTESIAN_POINT ( 'NONE',  ( 6.541171370350062020, -2.986177670315871335, 5.112746295475706582 ) ) ;
#13805 = ORIENTED_EDGE ( 'NONE', *, *, #2581, .T. ) ;
#13806 = EDGE_LOOP ( 'NONE', ( #13913, #8811, #1052, #7737 ) ) ;
#13807 = FILL_AREA_STYLE_COLOUR ( '', #7751 ) ;
#13808 = CARTESIAN_POINT ( 'NONE',  ( 229.2257385731836621, 308.4724102386199434, 182.7999999999996135 ) ) ;
#13809 = DIRECTION ( 'NONE',  ( 0.000000000000000000, 0.000000000000000000, -1.000000000000000000 ) ) ;
#13810 = CARTESIAN_POINT ( 'NONE',  ( 0.000000000000000000, 5.258101095580073669E-15, 4.000000000000000000 ) ) ;
#13811 = DIRECTION ( 'NONE',  ( 0.000000000000000000, 0.000000000000000000, 1.000000000000000000 ) ) ;
#13812 = VERTEX_POINT ( 'NONE', #10597 ) ;
#13813 = DIRECTION ( 'NONE',  ( 0.9578262852211525402, -0.2873478855663417764, 1.110223024625127747E-15 ) ) ;
#13814 = DIRECTION ( 'NONE',  ( -0.000000000000000000, -0.000000000000000000, -1.000000000000000000 ) ) ;
#13815 = DIRECTION ( 'NONE',  ( 0.000000000000000000, 0.000000000000000000, 1.000000000000000000 ) ) ;
#13816 = CARTESIAN_POINT ( 'NONE',  ( 6.466260427357663154, 2.904280683598005730, 5.030361703432624232 ) ) ;
#13817 = VERTEX_POINT ( 'NONE', #10519 ) ;
#13818 = ORIENTED_EDGE ( 'NONE', *, *, #6731, .T. ) ;
#13819 = LINE ( 'NONE', #1496, #7722 ) ;
#13820 = FACE_OUTER_BOUND ( 'NONE', #9916, .T. ) ;
#13821 = CARTESIAN_POINT ( 'NONE',  ( -3.528928113779633335, 5.468125903023623557, 1.037615360386517718E-15 ) ) ;
#13822 = EDGE_LOOP ( 'NONE', ( #9427, #12560, #4396, #8320 ) ) ;
#13823 = DIRECTION ( 'NONE',  ( -0.2873478855663452736, -0.9578262852211514300, 0.000000000000000000 ) ) ;
#13824 = CARTESIAN_POINT ( 'NONE',  ( 610.7462142612635034, 188.6189422762846561, -185.0840554379255707 ) ) ;
#13825 = EDGE_CURVE ( 'NONE', #9797, #4375, #387, .T. ) ;
#13826 = PLANE ( 'NONE',  #12018 ) ;
#13827 = EDGE_CURVE ( 'NONE', #293, #7278, #12657, .T. ) ;
#13828 = CARTESIAN_POINT ( 'NONE',  ( 455.5035746174796714, 294.6698471414878782, 210.0000000000000000 ) ) ;
#13829 = FACE_OUTER_BOUND ( 'NONE', #5706, .T. ) ;
#13830 = FACE_OUTER_BOUND ( 'NONE', #7839, .T. ) ;
#13831 = VERTEX_POINT ( 'NONE', #8379 ) ;
#13832 = CARTESIAN_POINT ( 'NONE',  ( -0.02448733951239248641, -4.877042772274742255, -3.751161874094027571 ) ) ;
#13833 = EDGE_LOOP ( 'NONE', ( #5727, #5860, #9338 ) ) ;
#13834 = ORIENTED_EDGE ( 'NONE', *, *, #880, .T. ) ;
#13835 = LINE ( 'NONE', #12729, #11335 ) ;
#13836 = CARTESIAN_POINT ( 'NONE',  ( 2.999999999999999112, 0.000000000000000000, 4.000000000000000000 ) ) ;
#13837 = CIRCLE ( 'NONE', #9836, 4.799999999999968736 ) ;
#13838 = LINE ( 'NONE', #7129, #6864 ) ;
#13839 = LINE ( 'NONE', #6307, #11717 ) ;
#13840 = ORIENTED_EDGE ( 'NONE', *, *, #1647, .F. ) ;
#13841 = CARTESIAN_POINT ( 'NONE',  ( 629.0000000000000000, 154.0000000000000284, -187.5000000000000000 ) ) ;
#13842 = EDGE_CURVE ( 'NONE', #14327, #10969, #3538, .T. ) ;
#13843 = CARTESIAN_POINT ( 'NONE',  ( 6.500000000000000888, -2.759515168581564204, -5.880113447610522570 ) ) ;
#13844 = CARTESIAN_POINT ( 'NONE',  ( -4.235886605889389145, -2.417314728048544303, -3.751161874094020909 ) ) ;
#13845 =( NAMED_UNIT ( * ) SI_UNIT ( $, .STERADIAN. ) SOLID_ANGLE_UNIT ( ) );
#13846 =( LENGTH_UNIT ( ) NAMED_UNIT ( * ) SI_UNIT ( .MILLI., .METRE. ) );
#13847 = ORIENTED_EDGE ( 'NONE', *, *, #683, .T. ) ;
#13848 = AXIS2_PLACEMENT_3D ( 'NONE', #11842, #1518, #11626 ) ;
#13849 = VECTOR ( 'NONE', #3657, 1000.000000000000000 ) ;
#13850 = ORIENTED_EDGE ( 'NONE', *, *, #3786, .F. ) ;
#13851 = ADVANCED_FACE ( 'NONE', ( #317 ), #260, .F. ) ;
#13852 = VECTOR ( 'NONE', #12559, 1000.000000000000227 ) ;
#13853 = ORIENTED_EDGE ( 'NONE', *, *, #8635, .T. ) ;
#13854 = PLANE ( 'NONE',  #12932 ) ;
#13855 =( REPRESENTATION_RELATIONSHIP ('NONE','NONE', #2822, #5462 ) REPRESENTATION_RELATIONSHIP_WITH_TRANSFORMATION ( #3965 )SHAPE_REPRESENTATION_RELATIONSHIP( ) );
#13856 = LINE ( 'NONE', #7950, #13906 ) ;
#13857 = LINE ( 'NONE', #9131, #12508 ) ;
#13858 =( GEOMETRIC_REPRESENTATION_CONTEXT ( 3 ) GLOBAL_UNCERTAINTY_ASSIGNED_CONTEXT ( ( #10942 ) ) GLOBAL_UNIT_ASSIGNED_CONTEXT ( ( #4299, #5541, #4519 ) ) REPRESENTATION_CONTEXT ( 'NONE', 'WORKASPACE' ) );
#13859 = VECTOR ( 'NONE', #9262, 1000.000000000000000 ) ;
#13860 = ORIENTED_EDGE ( 'NONE', *, *, #1270, .F. ) ;
#13861 = CARTESIAN_POINT ( 'NONE',  ( 0.01055556052339231068, -4.575665857285986959, -2.074714256722481220 ) ) ;
#13862 = EDGE_CURVE ( 'NONE', #9723, #3660, #905, .T. ) ;
#13863 = DIRECTION ( 'NONE',  ( 1.000000000000000000, 0.000000000000000000, 0.000000000000000000 ) ) ;
#13864 = DIRECTION ( 'NONE',  ( 1.000000000000000000, 0.000000000000000000, 0.000000000000000000 ) ) ;
#13865 = DIRECTION ( 'NONE',  ( 0.9578262852211513190, -0.2873478855663453846, 8.575812866481462478E-17 ) ) ;
#13866 = EDGE_LOOP ( 'NONE', ( #9034, #4588, #2995, #4099 ) ) ;
#13867 = CARTESIAN_POINT ( 'NONE',  ( 6.534838248920899595, 5.903531555104835071, -2.091255385257999292E-17 ) ) ;
#13868 = VERTEX_POINT ( 'NONE', #9639 ) ;
#13869 = ADVANCED_FACE ( 'NONE', ( #3147 ), #2345, .F. ) ;
#13870=STYLED_ITEM('',(#14667),#2617);
#13871 = EDGE_CURVE ( 'NONE', #2593, #7610, #4173, .T. ) ;
#13872 = DIRECTION ( 'NONE',  ( -0.000000000000000000, -0.000000000000000000, -1.000000000000000000 ) ) ;
#13873 = VECTOR ( 'NONE', #13095, 999.9999999999998863 ) ;
#13874 = AXIS2_PLACEMENT_3D ( 'NONE', #2221, #7977, #6728 ) ;
#13875 = ORIENTED_EDGE ( 'NONE', *, *, #7406, .T. ) ;
#13876 = ORIENTED_EDGE ( 'NONE', *, *, #1901, .T. ) ;
#13877 = CARTESIAN_POINT ( 'NONE',  ( 4.101954839143203912, -2.368264730583031330, -3.681130640444377988 ) ) ;
#13878 = LINE ( 'NONE', #13808, #4738 ) ;
#13879 = EDGE_CURVE ( 'NONE', #8002, #2622, #14144, .T. ) ;
#13880 = FACE_OUTER_BOUND ( 'NONE', #14294, .T. ) ;
#13881 = PRODUCT_DEFINITION ( 'UNKNOWN', '', #7844, #9461 ) ;
#13882 = DIRECTION ( 'NONE',  ( -1.000000000000000000, -0.000000000000000000, -0.000000000000000000 ) ) ;
#13883 = AXIS2_PLACEMENT_3D ( 'NONE', #6921, #11419, #5806 ) ;
#13884 = TOROIDAL_SURFACE ( 'NONE', #13177, 6.250000000000000000, 0.7500000000000000000 ) ;
#13885 = UNCERTAINTY_MEASURE_WITH_UNIT (LENGTH_MEASURE( 1.000000000000000082E-05 ), #12645, 'distance_accuracy_value', 'NONE');
#13886 = CARTESIAN_POINT ( 'NONE',  ( 641.0000000000000000, 166.0000000000000284, 187.5000000000000000 ) ) ;
#13887 = ORIENTED_EDGE ( 'NONE', *, *, #9085, .T. ) ;
#13888 = CYLINDRICAL_SURFACE ( 'NONE', #421, 7.000000000000000000 ) ;
#13889 = LINE ( 'NONE', #2597, #6327 ) ;
#13890 = DIRECTION ( 'NONE',  ( 0.000000000000000000, 0.000000000000000000, 1.000000000000000000 ) ) ;
#13891 = CIRCLE ( 'NONE', #1383, 6.500000000000000888 ) ;
#13892 = CARTESIAN_POINT ( 'NONE',  ( 6.506987859255518813, 2.925375531177291766, 5.066899051217865768 ) ) ;
#13893 = ORIENTED_EDGE ( 'NONE', *, *, #859, .T. ) ;
#13894 = ORIENTED_EDGE ( 'NONE', *, *, #5655, .T. ) ;
#13895 = CARTESIAN_POINT ( 'NONE',  ( 2.999999999999999112, 2.309401076758508253, 3.999999999999993339 ) ) ;
#13896 = DIRECTION ( 'NONE',  ( 0.000000000000000000, 0.000000000000000000, -1.000000000000000000 ) ) ;
#13897 = VECTOR ( 'NONE', #6660, 1000.000000000000000 ) ;
#13898 = AXIS2_PLACEMENT_3D ( 'NONE', #13120, #9800, #8901 ) ;
#13899 = DIRECTION ( 'NONE',  ( 1.000000000000000000, 0.000000000000000000, 0.000000000000000000 ) ) ;
#13900 = AXIS2_PLACEMENT_3D ( 'NONE', #5437, #2094, #1060 ) ;
#13901 = VERTEX_POINT ( 'NONE', #7351 ) ;
#13902 = EDGE_CURVE ( 'NONE', #10585, #8377, #8530, .T. ) ;
#13903 = DIRECTION ( 'NONE',  ( 0.000000000000000000, 1.000000000000000000, -1.224646799147353207E-16 ) ) ;
#13904 = CARTESIAN_POINT ( 'NONE',  ( 610.4513696044788276, 188.9932989497419555, -185.8927021017107677 ) ) ;
#13905 = CARTESIAN_POINT ( 'NONE',  ( 2.500000000000000000, 1.178949249685212974, -2.042000000000001148 ) ) ;
#13906 = VECTOR ( 'NONE', #6850, 1000.000000000000000 ) ;
#13907 = EDGE_CURVE ( 'NONE', #5137, #7551, #3070, .T. ) ;
#13908 = AXIS2_PLACEMENT_3D ( 'NONE', #4924, #3669, #3826 ) ;
#13909 = DIRECTION ( 'NONE',  ( -0.000000000000000000, -0.000000000000000000, 1.000000000000000000 ) ) ;
#13910 = CARTESIAN_POINT ( 'NONE',  ( 6.500000000000000000, -3.752776749732574135, -8.000000000000000000 ) ) ;
#13911 = DIRECTION ( 'NONE',  ( 0.000000000000000000, 0.000000000000000000, -1.000000000000000000 ) ) ;
#13912 = SURFACE_STYLE_USAGE ( .BOTH. , #371 ) ;
#13913 = ORIENTED_EDGE ( 'NONE', *, *, #2541, .T. ) ;
#13914 = CARTESIAN_POINT ( 'NONE',  ( 0.000000000000000000, 0.000000000000000000, -4.000000000000000000 ) ) ;
#13915 = ORIENTED_EDGE ( 'NONE', *, *, #1214, .F. ) ;
#13916 = ORIENTED_EDGE ( 'NONE', *, *, #12832, .F. ) ;
#13917 = VECTOR ( 'NONE', #8418, 1000.000000000000000 ) ;
#13918 = DIRECTION ( 'NONE',  ( -0.9578262852211525402, 0.2873478855663419429, 0.000000000000000000 ) ) ;
#13919 = VECTOR ( 'NONE', #7128, 1000.000000000000000 ) ;
#13920 = AXIS2_PLACEMENT_3D ( 'NONE', #14613, #10185, #3688 ) ;
#13921 = EDGE_CURVE ( 'NONE', #4085, #8737, #1802, .T. ) ;
#13922 = EDGE_CURVE ( 'NONE', #14108, #10070, #12917, .T. ) ;
#13923 = CARTESIAN_POINT ( 'NONE',  ( -0.2500000000000000000, -8.096141056083446585, -1.000000000000000000 ) ) ;
#13924 = VECTOR ( 'NONE', #14087, 1000.000000000000000 ) ;
#13925 = CARTESIAN_POINT ( 'NONE',  ( 237.7887055630606312, 337.0156335382089310, -182.8000000000007219 ) ) ;
#13926 = CARTESIAN_POINT ( 'NONE',  ( -9.999999999999998224, 376.8992337277234128, 187.0000000000000000 ) ) ;
#13927 = AXIS2_PLACEMENT_3D ( 'NONE', #12330, #13230, #13361 ) ;
#13928 = ORIENTED_EDGE ( 'NONE', *, *, #9713, .F. ) ;
#13929 = CARTESIAN_POINT ( 'NONE',  ( 3.510273485745307731, 2.827716139362654424, -3.610536846335885564 ) ) ;
#13930 = DIRECTION ( 'NONE',  ( 1.000000000000000000, 0.000000000000000000, -0.000000000000000000 ) ) ;
#13931 = VECTOR ( 'NONE', #5839, 1000.000000000000000 ) ;
#13932 = CARTESIAN_POINT ( 'NONE',  ( 6.270568613849412998, -3.932080789230356643, 3.401571648088637101 ) ) ;
#13933 = CARTESIAN_POINT ( 'NONE',  ( 628.0000000000000000, 235.0000000000000284, -263.5000000000000000 ) ) ;
#13934 = ORIENTED_EDGE ( 'NONE', *, *, #4778, .F. ) ;
#13935 = DIRECTION ( 'NONE',  ( -0.000000000000000000, -0.000000000000000000, 1.000000000000000000 ) ) ;
#13936 = ADVANCED_FACE ( 'NONE', ( #11984 ), #10895, .F. ) ;
#13937 = ORIENTED_EDGE ( 'NONE', *, *, #13484, .F. ) ;
#13939 = DIRECTION ( 'NONE',  ( -1.000000000000000000, 0.000000000000000000, 0.000000000000000000 ) ) ;
#13938 = AXIS2_PLACEMENT_3D ( 'NONE', #6944, #12556, #4820 ) ;
#13940 = EDGE_CURVE ( 'NONE', #2544, #3675, #9851, .T. ) ;
#13941 = VECTOR ( 'NONE', #11754, 1000.000000000000000 ) ;
#13942 = DIRECTION ( 'NONE',  ( 1.000000000000000000, 0.000000000000000000, 0.000000000000000000 ) ) ;
#13944 = DIRECTION ( 'NONE',  ( -1.000000000000000000, 0.000000000000000000, -0.000000000000000000 ) ) ;
#13943 = AXIS2_PLACEMENT_3D ( 'NONE', #6325, #14079, #8462 ) ;
#13945 = ORIENTED_EDGE ( 'NONE', *, *, #373, .T. ) ;
#13946 = CARTESIAN_POINT ( 'NONE',  ( 610.0000000000001137, 185.6790804732684990, 184.8000000000000966 ) ) ;
#13947 = DIRECTION ( 'NONE',  ( 0.2873478855663503806, 0.9578262852211499867, -3.544669318145085478E-17 ) ) ;
#13948 = CARTESIAN_POINT ( 'NONE',  ( 0.01055556052338863481, -4.084588180558399451, 2.925285743277528105 ) ) ;
#13949 = AXIS2_PLACEMENT_3D ( 'NONE', #2104, #10975, #8690 ) ;
#13950 = CARTESIAN_POINT ( 'NONE',  ( 4.000000000000000000, -2.309401076758516691, -0.4999999999999995559 ) ) ;
#13951 = ORIENTED_EDGE ( 'NONE', *, *, #1146, .F. ) ;
#13952 = VECTOR ( 'NONE', #2076, 1000.000000000000000 ) ;
#13953 = CARTESIAN_POINT ( 'NONE',  ( -4.000000000000000000, -0.8382240730041925492, -3.220610619767135141 ) ) ;
#13954 =( NAMED_UNIT ( * ) SI_UNIT ( $, .STERADIAN. ) SOLID_ANGLE_UNIT ( ) );
#13955 = ORIENTED_EDGE ( 'NONE', *, *, #10962, .F. ) ;
#13956 = DIRECTION ( 'NONE',  ( 1.000000000000000000, 0.000000000000000000, 0.000000000000000000 ) ) ;
#13957 = ORIENTED_EDGE ( 'NONE', *, *, #10871, .T. ) ;
#13958 = ORIENTED_EDGE ( 'NONE', *, *, #14296, .T. ) ;
#13959 = CARTESIAN_POINT ( 'NONE',  ( 628.0000000000000000, 152.9999999999999147, -225.5000000000000000 ) ) ;
#13960 = ADVANCED_FACE ( 'NONE', ( #8 ), #2086, .F. ) ;
#13961 = CARTESIAN_POINT ( 'NONE',  ( 6.385552186430388133, -2.886751345948119329, 5.000000000000000888 ) ) ;
#13962 = AXIS2_PLACEMENT_3D ( 'NONE', #13405, #7880, #2545 ) ;
#13963 = B_SPLINE_CURVE_WITH_KNOTS ( 'NONE', 3,
 ( #5995, #5775, #6885, #4829, #3572, #1277, #12635, #9168, #10348, #8127, #10278, #9322, #4897, #216, #137, #444, #4763, #9392 ),
 .UNSPECIFIED., .F., .F.,
 ( 4, 2, 2, 2, 2, 2, 2, 2, 4 ),
 ( 0.5000000000000000000, 0.5625000000000000000, 0.6250000000000000000, 0.6875000000000000000, 0.7500000000000000000, 0.8125000000000000000, 0.8750000000000000000, 0.9375000000000000000, 1.000000000000000000 ),
 .UNSPECIFIED. ) ;
#13964 = ADVANCED_FACE ( 'NONE', ( #5782 ), #8486, .F. ) ;
#13965 = DIRECTION ( 'NONE',  ( -9.498873539028489960E-17, 1.000000000000000000, 0.000000000000000000 ) ) ;
#13966 = PRODUCT_DEFINITION_SHAPE ( 'NONE', 'NONE',  #14622 ) ;
#13967 = CARTESIAN_POINT ( 'NONE',  ( 2.999999999999999112, 2.309401076758500704, -4.000000000000000000 ) ) ;
#13968 = EDGE_CURVE ( 'NONE', #5128, #5031, #10607, .T. ) ;
#13969 = DIRECTION ( 'NONE',  ( 0.2873478855663417764, 0.9578262852211525402, -6.938893903907204712E-15 ) ) ;
#13970 = ORIENTED_EDGE ( 'NONE', *, *, #2759, .T. ) ;
#13971 = ADVANCED_FACE ( 'NONE', ( #2169 ), #12970, .T. ) ;
#13972 = DIRECTION ( 'NONE',  ( 0.000000000000000000, 0.000000000000000000, 1.000000000000000000 ) ) ;
#13973 = LINE ( 'NONE', #5046, #8914 ) ;
#13974 = DIRECTION ( 'NONE',  ( 1.000000000000000000, 0.000000000000000000, 0.000000000000000000 ) ) ;
#13975 = AXIS2_PLACEMENT_3D ( 'NONE', #10017, #14457, #4272 ) ;
#13976 = LINE ( 'NONE', #9470, #13931 ) ;
#13977 = ORIENTED_EDGE ( 'NONE', *, *, #472, .F. ) ;
#13978 = ORIENTED_EDGE ( 'NONE', *, *, #2770, .F. ) ;
#13979 = CARTESIAN_POINT ( 'NONE',  ( 4.000000000000000000, -1.084202172485504434E-14, -3.142992957459231906 ) ) ;
#13980 = DIRECTION ( 'NONE',  ( 0.000000000000000000, 0.000000000000000000, -1.000000000000000000 ) ) ;
#13981 = PRODUCT_DEFINITION_FORMATION_WITH_SPECIFIED_SOURCE ( 'ANY', '', #11936, .NOT_KNOWN. ) ;
#13982 = CARTESIAN_POINT ( 'NONE',  ( -4.366061277241453098, 4.984806845751379889, -0.09463688534106590167 ) ) ;
#13983 = AXIS2_PLACEMENT_3D ( 'NONE', #9122, #2477, #3523 ) ;
#13984 = CYLINDRICAL_SURFACE ( 'NONE', #3530, 5.000000000000004441 ) ;
#13985 = EDGE_CURVE ( 'NONE', #3336, #12479, #3209, .T. ) ;
#13986 = EDGE_LOOP ( 'NONE', ( #5881, #13539, #6405, #9954 ) ) ;
#13987 = EDGE_CURVE ( 'NONE', #4931, #7500, #14379, .T. ) ;
#13988 = AXIS2_PLACEMENT_3D ( 'NONE', #4158, #10943, #6516 ) ;
#13989 = DIRECTION ( 'NONE',  ( -1.000000000000000000, -0.000000000000000000, -0.000000000000000000 ) ) ;
#13990 = CARTESIAN_POINT ( 'NONE',  ( 43.50000000000000711, 0.000000000000000000, 0.000000000000000000 ) ) ;
#13991 = CARTESIAN_POINT ( 'NONE',  ( 0.000000000000000000, 0.000000000000000000, 0.000000000000000000 ) ) ;
#13992 = EDGE_CURVE ( 'NONE', #11949, #3419, #5336, .T. ) ;
#13993 = CARTESIAN_POINT ( 'NONE',  ( -1.143494478793305150E-17, -0.3908539631446752427, -4.000000000000000000 ) ) ;
#13994 = PLANE ( 'NONE',  #12664 ) ;
#13995 = CARTESIAN_POINT ( 'NONE',  ( -4.211140560182196957, -2.431303136016552013, -3.745885042887436178 ) ) ;
#13996 = ORIENTED_EDGE ( 'NONE', *, *, #6432, .T. ) ;
#13997 = CARTESIAN_POINT ( 'NONE',  ( 1.243802165048773611, -3.900692638707475624, -3.223146290109810241 ) ) ;
#13998 = ORIENTED_EDGE ( 'NONE', *, *, #13235, .F. ) ;
#13999 = ORIENTED_EDGE ( 'NONE', *, *, #12669, .F. ) ;
#14000 =( GEOMETRIC_REPRESENTATION_CONTEXT ( 3 ) GLOBAL_UNCERTAINTY_ASSIGNED_CONTEXT ( ( #13016 ) ) GLOBAL_UNIT_ASSIGNED_CONTEXT ( ( #2393, #2238, #10144 ) ) REPRESENTATION_CONTEXT ( 'NONE', 'WORKASPACE' ) );
#14001 = DIRECTION ( 'NONE',  ( 0.000000000000000000, 0.000000000000000000, -1.000000000000000000 ) ) ;
#14002 = CLOSED_SHELL ( 'NONE', ( #8481, #1788, #52, #8133, #3019, #2588 ) ) ;
#14003 = DIRECTION ( 'NONE',  ( -1.000000000000000000, 0.000000000000000000, -0.000000000000000000 ) ) ;
#14004 = CARTESIAN_POINT ( 'NONE',  ( 0.04320752586819841951, 0.9836842030436123707, -5.000000000000000000 ) ) ;
#14005 = CARTESIAN_POINT ( 'NONE',  ( 636.7009106935324780, 155.5114698605638637, -211.0000000000000000 ) ) ;
#14006 = ORIENTED_EDGE ( 'NONE', *, *, #1525, .F. ) ;
#14007 = CARTESIAN_POINT ( 'NONE',  ( 2.804994570502171047, 3.229033611042449792, -3.526374918436834704 ) ) ;
#14008 = DIRECTION ( 'NONE',  ( 0.000000000000000000, 0.000000000000000000, 1.000000000000000000 ) ) ;
#14009 = CARTESIAN_POINT ( 'NONE',  ( 610.0000000000000000, 0.000000000000000000, -190.0000000000000000 ) ) ;
#14010 = FACE_OUTER_BOUND ( 'NONE', #9859, .T. ) ;
#14011 = VERTEX_POINT ( 'NONE', #76 ) ;
#14012 = CARTESIAN_POINT ( 'NONE',  ( 631.0000000000000000, 155.9999999999999432, -233.5000000000000000 ) ) ;
#14013 = CYLINDRICAL_SURFACE ( 'NONE', #1142, 2.649999999999985700 ) ;
#14014 = VERTEX_POINT ( 'NONE', #1123 ) ;
#14015 = CARTESIAN_POINT ( 'NONE',  ( 703.1581845006096501, 166.2926764603917036, 177.6000000000001648 ) ) ;
#14016 = CARTESIAN_POINT ( 'NONE',  ( 20.55500000000001748, 0.000000000000000000, 0.000000000000000000 ) ) ;
#14017 = LINE ( 'NONE', #14297, #5930 ) ;
#14018 = ORIENTED_EDGE ( 'NONE', *, *, #1975, .F. ) ;
#14019 = CARTESIAN_POINT ( 'NONE',  ( 609.7814593570623174, 185.8554382275811463, 186.1689414351991161 ) ) ;
#14020 = CARTESIAN_POINT ( 'NONE',  ( 629.0000000000000000, 154.0000000000000284, -187.5000000000000000 ) ) ;
#14021 = DIRECTION ( 'NONE',  ( -0.9237280213470676626, -0.3830490080632388272, 0.000000000000000000 ) ) ;
#14022 = CARTESIAN_POINT ( 'NONE',  ( 2.836893136758676270, 3.208949435745843903, -3.505054077164911241 ) ) ;
#14023 = EDGE_CURVE ( 'NONE', #3424, #6917, #4616, .T. ) ;
#14024 = VERTEX_POINT ( 'NONE', #7788 ) ;
#14025 = CARTESIAN_POINT ( 'NONE',  ( -4.000000000000000000, 1.677772373332757194, -3.535253723897187506 ) ) ;
#14026 = CARTESIAN_POINT ( 'NONE',  ( 642.0000000000000000, 153.0000000000000284, -233.5000000000000000 ) ) ;
#14027 = ORIENTED_EDGE ( 'NONE', *, *, #11960, .F. ) ;
#14028 = DIRECTION ( 'NONE',  ( 0.000000000000000000, 0.000000000000000000, -1.000000000000000000 ) ) ;
#14029 = ORIENTED_EDGE ( 'NONE', *, *, #13251, .F. ) ;
#14030 = DIRECTION ( 'NONE',  ( -0.9578262852211513190, 0.2873478855663453846, 0.000000000000000000 ) ) ;
#14031 = LINE ( 'NONE', #14178, #1866 ) ;
#14032 = CARTESIAN_POINT ( 'NONE',  ( 6.815830331203685866, 1.228021141713631082E-13, -6.171384342982610960 ) ) ;
#14033 = CARTESIAN_POINT ( 'NONE',  ( 641.0000000000000000, 154.0000000000000568, 187.5000000000000000 ) ) ;
#14034 = PRODUCT_DEFINITION_CONTEXT ( 'detailed design', #3296, 'design' ) ;
#14035 = B_SPLINE_CURVE_WITH_KNOTS ( 'NONE', 3,
 ( #438, #7171, #11445, #8410, #1337 ),
 .UNSPECIFIED., .F., .F.,
 ( 4, 1, 4 ),
 ( 5.644705275899819452E-20, 0.003752776749732567464, 0.007505553499465136662 ),
 .UNSPECIFIED. ) ;
#14036 = CARTESIAN_POINT ( 'NONE',  ( 142.4540310085880606, 355.9707293956415697, -190.0000000000000000 ) ) ;
#14037 = EDGE_CURVE ( 'NONE', #9599, #14014, #13606, .T. ) ;
#14038 = EDGE_LOOP ( 'NONE', ( #8932, #7011, #13375, #3252 ) ) ;
#14039 =( BOUNDED_SURFACE ( )  B_SPLINE_SURFACE ( 3, 2, ( 
 ( #11236, #11314, #3493 ),
 ( #12487, #2385, #12095 ),
 ( #4205, #14250, #4072 ),
 ( #8630, #6344, #5100 ),
 ( #11876, #8565, #7449 ),
 ( #10704, #5316, #3989 ) ),
 .UNSPECIFIED., .F., .F., .F. ) 
 B_SPLINE_SURFACE_WITH_KNOTS ( ( 4, 2, 4 ),
 ( 3, 3 ),
 ( 0.02367865728600888550, 0.02663179453327094853, 0.02958493178053300809 ),
 ( 0.000000000000000000, 1.000000000000000000 ),
 .UNSPECIFIED. ) 
 GEOMETRIC_REPRESENTATION_ITEM ( )  RATIONAL_B_SPLINE_SURFACE ( (
 ( 1.000000000000000000, 0.8047781103519414669, 1.000000000000000000),
 ( 1.000000000000000000, 0.8123785825980049946, 1.000000000000000000),
 ( 1.000000000000000000, 0.8190671539288042480, 1.000000000000000000),
 ( 1.000000000000000000, 0.8192352255335092481, 1.000000000000000000),
 ( 1.000000000000000000, 0.8126129676835899263, 1.000000000000000000),
 ( 1.000000000000000000, 0.8047712537969735624, 1.000000000000000000) ) ) 
 REPRESENTATION_ITEM ( '' )  SURFACE ( )  );
#14040 = CARTESIAN_POINT ( 'NONE',  ( 2.999999999999999112, 4.618802153517012954, 0.000000000000000000 ) ) ;
#14041 = CARTESIAN_POINT ( 'NONE',  ( 0.000000000000000000, 3.464101615137751278, -2.000000000000006217 ) ) ;
#14042 = DIRECTION ( 'NONE',  ( 1.000000000000000000, 0.000000000000000000, 0.000000000000000000 ) ) ;
#14043 = CARTESIAN_POINT ( 'NONE',  ( 6.385552186430388133, 2.886751345948125547, 4.999999999999999112 ) ) ;
#14044 = EDGE_LOOP ( 'NONE', ( #12639, #8582, #13203 ) ) ;
#14045 = EDGE_LOOP ( 'NONE', ( #8416, #8620, #10745, #5192 ) ) ;
#14046 = CARTESIAN_POINT ( 'NONE',  ( 635.0000000000000000, 235.0000000000000284, -233.5000000000000000 ) ) ;
#14047 = FACE_BOUND ( 'NONE', #4669, .T. ) ;
#14048 = EDGE_CURVE ( 'NONE', #2721, #5147, #7992, .T. ) ;
#14049 = PLANE ( 'NONE',  #3765 ) ;
#14050 = CARTESIAN_POINT ( 'NONE',  ( 0.000000000000000000, 0.000000000000000000, 2.700000000000000178 ) ) ;
#14051 = ORIENTED_EDGE ( 'NONE', *, *, #9158, .T. ) ;
#14052 = PLANE ( 'NONE',  #3383 ) ;
#14053 = CARTESIAN_POINT ( 'NONE',  ( 0.000000000000000000, 0.000000000000000000, 0.000000000000000000 ) ) ;
#14054 = LINE ( 'NONE', #11895, #8498 ) ;
#14055 = CARTESIAN_POINT ( 'NONE',  ( 459.3348797583642522, 272.6398425814014104, 210.0000000000000000 ) ) ;
#14056 = CARTESIAN_POINT ( 'NONE',  ( 164.3243839102495656, 402.9042173714779551, 190.0000000000000000 ) ) ;
#14057 = CARTESIAN_POINT ( 'NONE',  ( -0.6920835326022555245, -4.454600218803899558, -3.597382984111586079 ) ) ;
#14058 = ORIENTED_EDGE ( 'NONE', *, *, #5757, .T. ) ;
#14059 = DIRECTION ( 'NONE',  ( -1.000000000000000000, -0.000000000000000000, -0.000000000000000000 ) ) ;
#14060 = EDGE_LOOP ( 'NONE', ( #2178, #6654, #5980, #7004, #3353 ) ) ;
#14061 = ORIENTED_EDGE ( 'NONE', *, *, #7851, .F. ) ;
#14062 = LINE ( 'NONE', #3947, #12049 ) ;
#14063 = EDGE_CURVE ( 'NONE', #5539, #793, #10127, .T. ) ;
#14064 = ADVANCED_FACE ( 'NONE', ( #6682 ), #2301, .T. ) ;
#14065 = CARTESIAN_POINT ( 'NONE',  ( 470.8287951810180516, 310.9528939902474463, -190.0000000000000000 ) ) ;
#14066 = CARTESIAN_POINT ( 'NONE',  ( -5.065257024580716028E-16, 0.4887495715076925484, -5.000000000000000000 ) ) ;
#14067 = DIRECTION ( 'NONE',  ( 0.2873478855663470499, 0.9578262852211508749, 0.000000000000000000 ) ) ;
#14068 = EDGE_LOOP ( 'NONE', ( #13341, #13153, #9243, #10209 ) ) ;
#14069 = CARTESIAN_POINT ( 'NONE',  ( 448.9584422793565750, 264.0194060144110608, -210.0000000000000000 ) ) ;
#14070 = CYLINDRICAL_SURFACE ( 'NONE', #13908, 2.199999999999702194 ) ;
#14071 = CARTESIAN_POINT ( 'NONE',  ( -3.540020015735593439, -2.810662092924100630, -3.602146406945814672 ) ) ;
#14072 = CARTESIAN_POINT ( 'NONE',  ( 0.000000000000000000, 0.000000000000000000, -25.03750572909317285 ) ) ;
#14073 = VERTEX_POINT ( 'NONE', #11178 ) ;
#14074 = LINE ( 'NONE', #12966, #7517 ) ;
#14075 = ITEM_DEFINED_TRANSFORMATION ( 'NONE', 'NONE', #9958,  #9440 ) ;
#14076 = ORIENTED_EDGE ( 'NONE', *, *, #8437, .F. ) ;
#14077 = CARTESIAN_POINT ( 'NONE',  ( 446.3084422793565409, 264.0194060144110608, -210.0000000000000000 ) ) ;
#14078 = DIRECTION ( 'NONE',  ( 0.000000000000000000, 0.000000000000000000, 1.000000000000000000 ) ) ;
#14079 = DIRECTION ( 'NONE',  ( -0.000000000000000000, -0.000000000000000000, -1.000000000000000000 ) ) ;
#14080 = ORIENTED_EDGE ( 'NONE', *, *, #5409, .T. ) ;
#14081 = CARTESIAN_POINT ( 'NONE',  ( -4.000000000000000000, 4.898587196589412829E-16, -25.03750572909317285 ) ) ;
#14082 = VECTOR ( 'NONE', #6038, 1000.000000000000000 ) ;
#14083 = EDGE_CURVE ( 'NONE', #13629, #5518, #7710, .T. ) ;
#14084 = VECTOR ( 'NONE', #1558, 1000.000000000000000 ) ;
#14085 = CARTESIAN_POINT ( 'NONE',  ( -2.000000000000007550, -3.464101615137749945, 0.000000000000000000 ) ) ;
#14086 =( NAMED_UNIT ( * ) PLANE_ANGLE_UNIT ( ) SI_UNIT ( $, .RADIAN. ) );
#14087 = DIRECTION ( 'NONE',  ( 0.000000000000000000, 0.000000000000000000, -1.000000000000000000 ) ) ;
#14088 = ORIENTED_EDGE ( 'NONE', *, *, #9049, .F. ) ;
#14089 = EDGE_CURVE ( 'NONE', #689, #5458, #8238, .T. ) ;
#14090 = PRODUCT ( 'circlip for shafts normal_din_Circlip DIN 471 - 10 x 1', 'circlip for shafts normal_din_Circlip DIN 471 - 10 x 1', '', ( #14474 ) ) ;
#14091 = ORIENTED_EDGE ( 'NONE', *, *, #3511, .T. ) ;
#14092 = VERTEX_POINT ( 'NONE', #10062 ) ;
#14093 = DIRECTION ( 'NONE',  ( 0.000000000000000000, 0.000000000000000000, 1.000000000000000000 ) ) ;
#14094 = CIRCLE ( 'NONE', #167, 5.199999999999760369 ) ;
#14096 = LINE ( 'NONE', #11932, #13414 ) ;
#14095 = AXIS2_PLACEMENT_3D ( 'NONE', #2237, #10221, #6745 ) ;
#14097 = DIRECTION ( 'NONE',  ( -0.000000000000000000, -0.000000000000000000, 1.000000000000000000 ) ) ;
#14098 = EDGE_CURVE ( 'NONE', #3675, #10367, #10852, .T. ) ;
#14099 = DIRECTION ( 'NONE',  ( 1.000000000000000000, 0.000000000000000000, 0.000000000000000000 ) ) ;
#14100 = DIRECTION ( 'NONE',  ( -0.9237280213470676626, -0.3830490080632388272, 0.000000000000000000 ) ) ;
#14101 = ORIENTED_EDGE ( 'NONE', *, *, #11799, .F. ) ;
#14102 = CIRCLE ( 'NONE', #1130, 4.000000000000000000 ) ;
#14103 = VECTOR ( 'NONE', #535, 1000.000000000000000 ) ;
#14104 = CARTESIAN_POINT ( 'NONE',  ( 0.000000000000000000, 0.000000000000000000, -8.000000000000000000 ) ) ;
#14105 = CARTESIAN_POINT ( 'NONE',  ( 237.7887055630607733, 337.0156335382104089, 179.7999999999995850 ) ) ;
#14106 = DIRECTION ( 'NONE',  ( 1.000000000000000000, 0.000000000000000000, 0.000000000000000000 ) ) ;
#14107 = CARTESIAN_POINT ( 'NONE',  ( -1.500000000000001332, 0.000000000000000000, -7.399999999999999467 ) ) ;
#14108 = VERTEX_POINT ( 'NONE', #6743 ) ;
#14109 = ORIENTED_EDGE ( 'NONE', *, *, #9512, .T. ) ;
#14110 = DIRECTION ( 'NONE',  ( -1.000000000000000000, 0.000000000000000000, 0.000000000000000000 ) ) ;
#14111 = LINE ( 'NONE', #295, #13497 ) ;
#14112 = CARTESIAN_POINT ( 'NONE',  ( 610.0000000000001137, 191.1080398579018720, -190.0000000000000000 ) ) ;
#14113 = EDGE_CURVE ( 'NONE', #6071, #11023, #11242, .T. ) ;
#14114 = PRESENTATION_LAYER_ASSIGNMENT (  '', '', ( #13870 ) ) ;
#14115 = VECTOR ( 'NONE', #13591, 1000.000000000000227 ) ;
#14116 = DIRECTION ( 'NONE',  ( -1.000000000000000000, -0.000000000000000000, -0.000000000000000000 ) ) ;
#14117 = ORIENTED_EDGE ( 'NONE', *, *, #13792, .T. ) ;
#14118 = CARTESIAN_POINT ( 'NONE',  ( 10.00000000000000000, 10.00000000000000178, -210.0000000000000000 ) ) ;
#14119 = CARTESIAN_POINT ( 'NONE',  ( -6.473970235329672780E-16, -4.862606272033106691, -3.745885042887442395 ) ) ;
#14120 = CARTESIAN_POINT ( 'NONE',  ( 639.4338945024659324, 161.8386352387035743, -210.0000000000000000 ) ) ;
#14121 = COLOUR_RGB ( '',0.8941176470588234615, 0.8941176470588234615, 0.8941176470588234615 ) ;
#14122 = DIRECTION ( 'NONE',  ( -0.000000000000000000, -0.000000000000000000, -1.000000000000000000 ) ) ;
#14123 = CARTESIAN_POINT ( 'NONE',  ( 1.567478505476134803E-15, 4.618802153517012954, -3.504269196027872457 ) ) ;
#14124 = CARTESIAN_POINT ( 'NONE',  ( 590.0000000000000000, 0.000000000000000000, 210.0000000000000000 ) ) ;
#14125 = ORIENTED_EDGE ( 'NONE', *, *, #11342, .F. ) ;
#14126 = AXIS2_PLACEMENT_3D ( 'NONE', #10567, #448, #1345 ) ;
#14127 = DIRECTION ( 'NONE',  ( 0.000000000000000000, 0.000000000000000000, -1.000000000000000000 ) ) ;
#14128 = VECTOR ( 'NONE', #5177, 1000.000000000000000 ) ;
#14129 = VERTEX_POINT ( 'NONE', #12800 ) ;
#14130 = ORIENTED_EDGE ( 'NONE', *, *, #8864, .T. ) ;
#14131 = FACE_OUTER_BOUND ( 'NONE', #2009, .T. ) ;
#14132 = EDGE_CURVE ( 'NONE', #7721, #14191, #2829, .T. ) ;
#14133 = AXIS2_PLACEMENT_3D ( 'NONE', #6537, #4398, #778 ) ;
#14134 = CARTESIAN_POINT ( 'NONE',  ( -5.357619327558936585E-16, 7.505553499465137612, -8.000000000000000000 ) ) ;
#14135 = DIRECTION ( 'NONE',  ( 0.000000000000000000, 0.000000000000000000, 1.000000000000000000 ) ) ;
#14136 = EDGE_CURVE ( 'NONE', #4166, #5188, #3779, .T. ) ;
#14137 = VECTOR ( 'NONE', #2443, 1000.000000000000000 ) ;
#14138 = PLANE ( 'NONE',  #4419 ) ;
#14139 = VECTOR ( 'NONE', #9738, 1000.000000000000227 ) ;
#14140 = EDGE_LOOP ( 'NONE', ( #6733, #8889 ) ) ;
#14141 = EDGE_CURVE ( 'NONE', #10969, #5056, #7068, .T. ) ;
#14142 = FACE_OUTER_BOUND ( 'NONE', #12795, .T. ) ;
#14143 =( REPRESENTATION_RELATIONSHIP ('NONE','NONE', #2822, #1780 ) REPRESENTATION_RELATIONSHIP_WITH_TRANSFORMATION ( #9857 )SHAPE_REPRESENTATION_RELATIONSHIP( ) );
#14144 = LINE ( 'NONE', #9931, #14611 ) ;
#14145 = EDGE_CURVE ( 'NONE', #9301, #6798, #1566, .T. ) ;
#14146 = CARTESIAN_POINT ( 'NONE',  ( 0.02511973781850649831, -4.877415612947427981, -3.751298745799844792 ) ) ;
#14147 = DIRECTION ( 'NONE',  ( 1.000000000000000000, 0.000000000000000000, 0.000000000000000000 ) ) ;
#14148 = VERTEX_POINT ( 'NONE', #11741 ) ;
#14149 = CIRCLE ( 'NONE', #6836, 2.649999999999985700 ) ;
#14150 = ADVANCED_FACE ( 'NONE', ( #13686 ), #10358, .T. ) ;
#14151 = CARTESIAN_POINT ( 'NONE',  ( -4.336808689942017736E-16, 7.505553499465137612, -0.8000000000000003775 ) ) ;
#14152 = CARTESIAN_POINT ( 'NONE',  ( 610.6325945170714249, 188.6953700521320911, 185.3721572044278787 ) ) ;
#14153 = ORIENTED_EDGE ( 'NONE', *, *, #2207, .T. ) ;
#14154 = VECTOR ( 'NONE', #9214, 1000.000000000000000 ) ;
#14155 = AXIS2_PLACEMENT_3D ( 'NONE', #8962, #13469, #7867 ) ;
#14156 = CARTESIAN_POINT ( 'NONE',  ( 2.500000000000000000, -2.357898499370432166, 3.035766082959412415E-15 ) ) ;
#14157 = CARTESIAN_POINT ( 'NONE',  ( 6.831979103402612274, 3.295157223185832596, -6.443785395948806283 ) ) ;
#14158 = VECTOR ( 'NONE', #7162, 1000.000000000000114 ) ;
#14159 = VECTOR ( 'NONE', #14324, 1000.000000000000114 ) ;
#14160 = DIRECTION ( 'NONE',  ( 0.000000000000000000, 0.000000000000000000, 1.000000000000000000 ) ) ;
#14161 = ORIENTED_EDGE ( 'NONE', *, *, #10871, .F. ) ;
#14162 = CARTESIAN_POINT ( 'NONE',  ( 629.0000000000000000, 166.0000000000000284, 187.5000000000000000 ) ) ;
#14163 = CARTESIAN_POINT ( 'NONE',  ( 0.000000000000000000, 0.000000000000000000, 0.000000000000000000 ) ) ;
#14164 = ADVANCED_FACE ( 'NONE', ( #11610, #6964 ), #8072, .T. ) ;
#14165 = VECTOR ( 'NONE', #12651, 1000.000000000000000 ) ;
#14166 = ADVANCED_FACE ( 'NONE', ( #6002 ), #4836, .F. ) ;
#14167 = AXIS2_PLACEMENT_3D ( 'NONE', #7409, #2912, #1857 ) ;
#14168 = CARTESIAN_POINT ( 'NONE',  ( 610.2669374424701800, 189.5106555248625284, -186.4579326193729969 ) ) ;
#14169 = CARTESIAN_POINT ( 'NONE',  ( -8.505790995055079406, 376.6597771564183859, 190.0000000000000284 ) ) ;
#14170 = ORIENTED_EDGE ( 'NONE', *, *, #6401, .F. ) ;
#14171 =( NAMED_UNIT ( * ) PLANE_ANGLE_UNIT ( ) SI_UNIT ( $, .RADIAN. ) );
#14172 = ORIENTED_EDGE ( 'NONE', *, *, #4847, .T. ) ;
#14173 = VECTOR ( 'NONE', #1549, 1000.000000000000114 ) ;
#14174 = CONICAL_SURFACE ( 'NONE', #1439, 5.000000000000000888, 1.047197551196600296 ) ;
#14175 = ORIENTED_EDGE ( 'NONE', *, *, #8157, .F. ) ;
#14176 = CARTESIAN_POINT ( 'NONE',  ( 2.999999999999999112, 0.000000000000000000, 0.000000000000000000 ) ) ;
#14177 = EDGE_CURVE ( 'NONE', #14270, #4614, #12576, .T. ) ;
#14178 = CARTESIAN_POINT ( 'NONE',  ( 101.4713065522757063, 338.2376885075856876, -169.9999999999999716 ) ) ;
#14179 = CARTESIAN_POINT ( 'NONE',  ( 641.0061384268468601, 164.6003227093606540, -210.0000000000000000 ) ) ;
#14180 = EDGE_CURVE ( 'NONE', #488, #6919, #4637, .T. ) ;
#14181 = CARTESIAN_POINT ( 'NONE',  ( 3.500000000000000000, -4.618802153516999631, 0.000000000000000000 ) ) ;
#14182 = CIRCLE ( 'NONE', #11576, 5.199999999999999289 ) ;
#14183 = UNCERTAINTY_MEASURE_WITH_UNIT (LENGTH_MEASURE( 1.000000000000000082E-05 ), #13240, 'distance_accuracy_value', 'NONE');
#14184 = CARTESIAN_POINT ( 'NONE',  ( 631.0000000000000000, 155.9999999999999432, -225.5000000000000000 ) ) ;
#14185 = ORIENTED_EDGE ( 'NONE', *, *, #8539, .T. ) ;
#14186 = CARTESIAN_POINT ( 'NONE',  ( 7.240873133980832321, 470.9098836221799047, -190.0000000000001990 ) ) ;
#14187 = PLANE ( 'NONE',  #11051 ) ;
#14188 = DIRECTION ( 'NONE',  ( 0.000000000000000000, 0.000000000000000000, -1.000000000000000000 ) ) ;
#14189 = FACE_OUTER_BOUND ( 'NONE', #7806, .T. ) ;
#14190 = ORIENTED_EDGE ( 'NONE', *, *, #9016, .F. ) ;
#14191 = VERTEX_POINT ( 'NONE', #13762 ) ;
#14192 = TOROIDAL_SURFACE ( 'NONE', #5703, 7.399999999999999467, 0.1000000000000000472 ) ;
#14193 = CARTESIAN_POINT ( 'NONE',  ( 635.0000000000000000, 160.0000000000000284, -210.0000000000000000 ) ) ;
#14194 = DIRECTION ( 'NONE',  ( 0.000000000000000000, 0.000000000000000000, -1.000000000000000000 ) ) ;
#14195 = CARTESIAN_POINT ( 'NONE',  ( -3.250000000000000444, -5.629165124598859649, -5.592027715088708995 ) ) ;
#14196 =( GEOMETRIC_REPRESENTATION_CONTEXT ( 3 ) GLOBAL_UNCERTAINTY_ASSIGNED_CONTEXT ( ( #11656 ) ) GLOBAL_UNIT_ASSIGNED_CONTEXT ( ( #13305, #14555, #8945 ) ) REPRESENTATION_CONTEXT ( 'NONE', 'WORKASPACE' ) );
#14197 = LINE ( 'NONE', #8581, #10828 ) ;
#14198 = ORIENTED_EDGE ( 'NONE', *, *, #5498, .T. ) ;
#14199 = VECTOR ( 'NONE', #8322, 1000.000000000000000 ) ;
#14200 = CARTESIAN_POINT ( 'NONE',  ( 137.1540310085880776, 355.9707293956415697, -190.0000000000000000 ) ) ;
#14201 = CARTESIAN_POINT ( 'NONE',  ( 0.9108756637626340691, 6.979659189792313256, -6.219623095964331050 ) ) ;
#14202 = DIRECTION ( 'NONE',  ( 0.000000000000000000, 0.000000000000000000, -1.000000000000000000 ) ) ;
#14203 = VERTEX_POINT ( 'NONE', #6076 ) ;
#14204 = DIRECTION ( 'NONE',  ( 1.000000000000000000, 0.000000000000000000, -0.000000000000000000 ) ) ;
#14205 = CARTESIAN_POINT ( 'NONE',  ( -6.269955739554009533, -4.268932597852945321, -6.443844059477445541 ) ) ;
#14206 = PLANE ( 'NONE',  #7974 ) ;
#14207 =( LENGTH_UNIT ( ) NAMED_UNIT ( * ) SI_UNIT ( .MILLI., .METRE. ) );
#14208 = PRODUCT_DEFINITION_SHAPE ( 'NONE', 'NONE',  #14636 ) ;
#14209 = EDGE_CURVE ( 'NONE', #8096, #5188, #4906, .T. ) ;
#14210 = ORIENTED_EDGE ( 'NONE', *, *, #1769, .F. ) ;
#14211 = FACE_OUTER_BOUND ( 'NONE', #12143, .T. ) ;
#14212 = DIRECTION ( 'NONE',  ( 0.000000000000000000, 0.000000000000000000, -1.000000000000000000 ) ) ;
#14213 = ORIENTED_EDGE ( 'NONE', *, *, #3376, .F. ) ;
#14214 = ORIENTED_EDGE ( 'NONE', *, *, #13247, .T. ) ;
#14215 = CARTESIAN_POINT ( 'NONE',  ( 2.500000000000000000, 1.768423874527823791, 1.020999999999998353 ) ) ;
#14216 = AXIS2_PLACEMENT_3D ( 'NONE', #14301, #1903, #1009 ) ;
#14217 = CARTESIAN_POINT ( 'NONE',  ( 1.567478505476134606E-15, 4.618802153517012066, -5.000000000000000000 ) ) ;
#14218 = EDGE_LOOP ( 'NONE', ( #5246, #9382, #8834, #9776, #8146 ) ) ;
#14219 = ORIENTED_EDGE ( 'NONE', *, *, #3968, .T. ) ;
#14220 = CARTESIAN_POINT ( 'NONE',  ( 628.4466020873430807, 163.7771423527818229, 210.0000119999999981 ) ) ;
#14221 = CARTESIAN_POINT ( 'NONE',  ( 451.6722694765949768, 316.6998517015743460, 210.0000000000000000 ) ) ;
#14222 = CARTESIAN_POINT ( 'NONE',  ( 0.000000000000000000, 0.000000000000000000, 0.000000000000000000 ) ) ;
#14223 = FILL_AREA_STYLE_COLOUR ( '', #13710 ) ;
#14224 = AXIS2_PLACEMENT_3D ( 'NONE', #774, #5221, #2994 ) ;
#14225 = EDGE_CURVE ( 'NONE', #12905, #9276, #4985, .T. ) ;
#14226 = ORIENTED_EDGE ( 'NONE', *, *, #8539, .F. ) ;
#14227 = CLOSED_SHELL ( 'NONE', ( #14399, #9083, #1696, #5678, #11205, #7621, #3592, #13756, #6003, #1023, #10757, #14353, #1874, #13314, #401, #7626, #8667, #12888, #9355, #8729, #1849, #7733, #7467, #11101, #318, #8546, #8801, #3447, #5057 ) ) ;
#14228 = DIRECTION ( 'NONE',  ( -0.2873478855663452736, -0.9578262852211514300, 0.000000000000000000 ) ) ;
#14229 = DIRECTION ( 'NONE',  ( 1.000000000000000000, 0.000000000000000000, 0.000000000000000000 ) ) ;
#14230 = ORIENTED_EDGE ( 'NONE', *, *, #10181, .T. ) ;
#14231 = EDGE_CURVE ( 'NONE', #3145, #992, #10438, .T. ) ;
#14232 = ORIENTED_EDGE ( 'NONE', *, *, #427, .T. ) ;
#14233 = ADVANCED_FACE ( 'NONE', ( #5938, #301 ), #13826, .T. ) ;
#14234 = CARTESIAN_POINT ( 'NONE',  ( 703.1581845006096501, 166.2926764603917036, -149.9999999999986642 ) ) ;
#14235 = FACE_BOUND ( 'NONE', #7801, .T. ) ;
#14236 = ADVANCED_FACE ( 'NONE', ( #12718 ), #9911, .T. ) ;
#14237 = VERTEX_POINT ( 'NONE', #3879 ) ;
#14238 = CARTESIAN_POINT ( 'NONE',  ( 5.200000000000002842, 0.000000000000000000, 0.000000000000000000 ) ) ;
#14239 = DIRECTION ( 'NONE',  ( 0.000000000000000000, 0.000000000000000000, 1.000000000000000000 ) ) ;
#14240 = DIRECTION ( 'NONE',  ( 0.2873478855663453291, 0.9578262852211513190, 0.000000000000000000 ) ) ;
#14241 = VERTEX_POINT ( 'NONE', #5272 ) ;
#14242 = CARTESIAN_POINT ( 'NONE',  ( 145.1678582058265192, 408.6511750828049117, 210.0000000000000000 ) ) ;
#14243 =( LENGTH_UNIT ( ) NAMED_UNIT ( * ) SI_UNIT ( .MILLI., .METRE. ) );
#14244 = ORIENTED_EDGE ( 'NONE', *, *, #88, .F. ) ;
#14245 = EDGE_LOOP ( 'NONE', ( #13286, #6961, #14355, #7589 ) ) ;
#14246 = LINE ( 'NONE', #4353, #4211 ) ;
#14247 = EDGE_CURVE ( 'NONE', #3772, #8326, #4424, .T. ) ;
#14248 = EDGE_CURVE ( 'NONE', #13718, #12356, #11490, .T. ) ;
#14249 = CARTESIAN_POINT ( 'NONE',  ( 3.309651814758564736, -5.455921364805393026, -1.000000000000000000 ) ) ;
#14250 = CARTESIAN_POINT ( 'NONE',  ( 6.207530437345012864, 4.849805425594809094, -1.599890596046773084 ) ) ;
#14251 = EDGE_CURVE ( 'NONE', #6798, #6803, #14269, .T. ) ;
#14252 = VECTOR ( 'NONE', #10539, 1000.000000000000114 ) ;
#14253 = DIRECTION ( 'NONE',  ( 0.000000000000000000, -0.5000000000000013323, -0.8660254037844380415 ) ) ;
#14254 = DIRECTION ( 'NONE',  ( -1.000000000000000000, -6.938893903907222067E-15, 0.000000000000000000 ) ) ;
#14255 = ORIENTED_EDGE ( 'NONE', *, *, #8744, .T. ) ;
#14256 = PLANE ( 'NONE',  #6058 ) ;
#14257 = CARTESIAN_POINT ( 'NONE',  ( 0.03421028094653150164, 3.072372537026367478, -2.678494666091042475 ) ) ;
#14258 = CARTESIAN_POINT ( 'NONE',  ( 139.8040310085880833, 355.9707293956415697, -215.0000000000000000 ) ) ;
#14259 = LINE ( 'NONE', #9894, #479 ) ;
#14260 = ORIENTED_EDGE ( 'NONE', *, *, #764, .T. ) ;
#14261 = ORIENTED_EDGE ( 'NONE', *, *, #9307, .T. ) ;
#14262 = CARTESIAN_POINT ( 'NONE',  ( 635.0000000000000000, 235.0000000000000284, -225.5000000000000000 ) ) ;
#14263 = CARTESIAN_POINT ( 'NONE',  ( 8.500000000000000000, 4.898587196589412829E-16, -4.000000000000000000 ) ) ;
#14264 = CARTESIAN_POINT ( 'NONE',  ( 609.7983275391768530, 185.9141716657875349, -186.1519484124941641 ) ) ;
#14265 = CARTESIAN_POINT ( 'NONE',  ( 6.500000000000000000, -3.752776749732574135, -6.064240316920400886 ) ) ;
#14266 = ORIENTED_EDGE ( 'NONE', *, *, #10253, .T. ) ;
#14267 = B_SPLINE_CURVE_WITH_KNOTS ( 'NONE', 3,
 ( #4215, #2131, #4144, #12025, #803 ),
 .UNSPECIFIED., .F., .F.,
 ( 4, 1, 4 ),
 ( 0.000000000000000000, 0.002886751345948128985, 0.005773502691896257970 ),
 .UNSPECIFIED. ) ;
#14268 = CARTESIAN_POINT ( 'NONE',  ( -6.500000000000000888, 4.076783350660894811, -6.121918786669029444 ) ) ;
#14269 = LINE ( 'NONE', #6227, #7314 ) ;
#14270 = VERTEX_POINT ( 'NONE', #10877 ) ;
#14271 = CARTESIAN_POINT ( 'NONE',  ( 229.2257385731836905, 308.4724102386184654, -179.8000000000005230 ) ) ;
#14272 = LINE ( 'NONE', #2831, #6343 ) ;
#14273 = DIRECTION ( 'NONE',  ( -0.9578262852211514300, 0.2873478855663454401, 0.000000000000000000 ) ) ;
#14274 = PRESENTATION_STYLE_ASSIGNMENT (( #7636 ) ) ;
#14275 = VERTEX_POINT ( 'NONE', #10794 ) ;
#14276 = PLANE ( 'NONE',  #9904 ) ;
#14277 = ORIENTED_EDGE ( 'NONE', *, *, #7472, .T. ) ;
#14278 = ORIENTED_EDGE ( 'NONE', *, *, #6816, .F. ) ;
#14279 = CARTESIAN_POINT ( 'NONE',  ( 0.4465819873851995525, 2.886751345948122882, -5.000000000000000000 ) ) ;
#14280 = CARTESIAN_POINT ( 'NONE',  ( 0.000000000000000000, 0.000000000000000000, 0.000000000000000000 ) ) ;
#14281 = EDGE_CURVE ( 'NONE', #5236, #11328, #6445, .T. ) ;
#14282 = ORIENTED_EDGE ( 'NONE', *, *, #5240, .F. ) ;
#14283 = ADVANCED_FACE ( 'NONE', ( #7748 ), #669, .T. ) ;
#14284 = EDGE_LOOP ( 'NONE', ( #5946, #1373, #13736, #628 ) ) ;
#14285 = DIRECTION ( 'NONE',  ( 1.000000000000000000, 0.000000000000000000, 0.000000000000000000 ) ) ;
#14286 = CARTESIAN_POINT ( 'NONE',  ( 6.500000000000000888, 2.723353699433710862, -5.896365680526115760 ) ) ;
#14287 = DIRECTION ( 'NONE',  ( 1.000000000000000000, 0.000000000000000000, 0.000000000000000000 ) ) ;
#14288 = CARTESIAN_POINT ( 'NONE',  ( -1.500000000000001332, 8.541911424052788811E-16, 6.975000000000000533 ) ) ;
#14289 = ORIENTED_EDGE ( 'NONE', *, *, #7432, .T. ) ;
#14290 = CARTESIAN_POINT ( 'NONE',  ( 610.0000000000001137, 185.6790804732684705, 184.8000000000000398 ) ) ;
#14291 = DIRECTION ( 'NONE',  ( 0.000000000000000000, 0.000000000000000000, -1.000000000000000000 ) ) ;
#14292 = VERTEX_POINT ( 'NONE', #14120 ) ;
#14293 = CARTESIAN_POINT ( 'NONE',  ( 609.9999999999998863, 227.4403065089098277, 184.7999999999999829 ) ) ;
#14294 = EDGE_LOOP ( 'NONE', ( #2983, #4629, #12140 ) ) ;
#14295 = DIRECTION ( 'NONE',  ( 0.000000000000000000, 0.000000000000000000, 1.000000000000000000 ) ) ;
#14296 = EDGE_CURVE ( 'NONE', #2721, #12114, #2362, .T. ) ;
#14297 = CARTESIAN_POINT ( 'NONE',  ( 2.999999999999999112, -2.309401076758502480, -4.000000000000000000 ) ) ;
#14298 = ORIENTED_EDGE ( 'NONE', *, *, #5808, .T. ) ;
#14299 = CARTESIAN_POINT ( 'NONE',  ( 610.0000000000001137, 191.1080398579019572, 186.9697000000000173 ) ) ;
#14300 = CARTESIAN_POINT ( 'NONE',  ( 0.000000000000000000, 0.000000000000000000, -4.484454397937119197 ) ) ;
#14301 = CARTESIAN_POINT ( 'NONE',  ( 635.0000000000000000, 160.0000000000000284, 207.0000000000000000 ) ) ;
#14302 = DIRECTION ( 'NONE',  ( 0.000000000000000000, 0.000000000000000000, 1.000000000000000000 ) ) ;
#14303 = VERTEX_POINT ( 'NONE', #10727 ) ;
#14304 = EDGE_CURVE ( 'NONE', #10035, #3502, #2827, .T. ) ;
#14305 = LINE ( 'NONE', #795, #6070 ) ;
#14306 = EDGE_LOOP ( 'NONE', ( #4379, #6839, #12404, #9448 ) ) ;
#14307 = ORIENTED_EDGE ( 'NONE', *, *, #3066, .T. ) ;
#14308 = CARTESIAN_POINT ( 'NONE',  ( 0.000000000000000000, 3.464101615137752610, 2.000000000000003997 ) ) ;
#14309 = CARTESIAN_POINT ( 'NONE',  ( 9.573736116531104419E-16, -7.693917458112909280, -6.460793508093584769 ) ) ;
#14310 = ADVANCED_FACE ( 'NONE', ( #3322 ), #534, .F. ) ;
#14311 = CARTESIAN_POINT ( 'NONE',  ( 642.5000000000001137, 160.0000000000000284, -210.0000059999999849 ) ) ;
#14312 = VECTOR ( 'NONE', #11066, 1000.000000000000000 ) ;
#14313 = VECTOR ( 'NONE', #10514, 1000.000000000000000 ) ;
#14314 = LINE ( 'NONE', #8704, #9920 ) ;
#14315 = UNCERTAINTY_MEASURE_WITH_UNIT (LENGTH_MEASURE( 1.000000000000000082E-05 ), #2373, 'distance_accuracy_value', 'NONE');
#14316 = CARTESIAN_POINT ( 'NONE',  ( 723.8855453127953297, 217.2873478855664757, 177.5999999999999659 ) ) ;
#14317 = EDGE_CURVE ( 'NONE', #8096, #1135, #12939, .T. ) ;
#14318 = ORIENTED_EDGE ( 'NONE', *, *, #1821, .T. ) ;
#14319 = ADVANCED_FACE ( 'NONE', ( #7827 ), #5060, .F. ) ;
#14320 = LINE ( 'NONE', #3244, #14312 ) ;
#14321 = CARTESIAN_POINT ( 'NONE',  ( 1.400000000000001910, 0.000000000000000000, -5.000000000000000000 ) ) ;
#14322 = B_SPLINE_CURVE_WITH_KNOTS ( 'NONE', 3,
 ( #3559, #11587, #9311, #9153 ),
 .UNSPECIFIED., .F., .F.,
 ( 4, 4 ),
 ( 2.380737581618690687E-07, 0.002336974151641533874 ),
 .UNSPECIFIED. ) ;
#14323 = CIRCLE ( 'NONE', #11477, 4.199999999999981526 ) ;
#14325 = EDGE_CURVE ( 'NONE', #9335, #1236, #14054, .T. ) ;
#14324 = DIRECTION ( 'NONE',  ( -0.9578262852211489875, 0.2873478855663534892, 0.000000000000000000 ) ) ;
#14326 = CONICAL_SURFACE ( 'NONE', #875, 8.542937654374687995, 1.221730476396047926 ) ;
#14327 = VERTEX_POINT ( 'NONE', #7329 ) ;
#14328 = EDGE_LOOP ( 'NONE', ( #187, #13315, #14414, #6424 ) ) ;
#14329 = CARTESIAN_POINT ( 'NONE',  ( 443.6584422793565636, 264.0194060144110608, 190.0000000000000000 ) ) ;
#14330 = CARTESIAN_POINT ( 'NONE',  ( 451.6722694765949768, 316.6998517015743460, -210.0000000000000000 ) ) ;
#14331 = CARTESIAN_POINT ( 'NONE',  ( 6.507056315241515954, 5.826803161468471437, -0.09231912136634902455 ) ) ;
#14332 = APPLICATION_CONTEXT ( 'automotive_design' ) ;
#14333 = CARTESIAN_POINT ( 'NONE',  ( -6.725979247667768668, 3.622307570260310694, -6.470294263593358686 ) ) ;
#14335 = ORIENTED_EDGE ( 'NONE', *, *, #13466, .T. ) ;
#14334 = AXIS2_PLACEMENT_3D ( 'NONE', #14262, #9826, #9544 ) ;
#14336 = VECTOR ( 'NONE', #13909, 1000.000000000000000 ) ;
#14337 = CARTESIAN_POINT ( 'NONE',  ( -6.500000000000000888, -1.360915494584213459, -5.718331000733963165 ) ) ;
#14338 = ORIENTED_EDGE ( 'NONE', *, *, #9890, .F. ) ;
#14339 = DIRECTION ( 'NONE',  ( -1.000000000000000000, -0.000000000000000000, -0.000000000000000000 ) ) ;
#14340 = DIRECTION ( 'NONE',  ( 0.000000000000000000, 0.000000000000000000, 1.000000000000000000 ) ) ;
#14341 = LINE ( 'NONE', #4235, #3505 ) ;
#14342 = ORIENTED_EDGE ( 'NONE', *, *, #10655, .F. ) ;
#14343 = CARTESIAN_POINT ( 'NONE',  ( 610.0000000000000000, 145.0000000000000568, -210.0000000000000000 ) ) ;
#14344 = ORIENTED_EDGE ( 'NONE', *, *, #8786, .T. ) ;
#14345 = ORIENTED_EDGE ( 'NONE', *, *, #5863, .F. ) ;
#14346 = CARTESIAN_POINT ( 'NONE',  ( 0.01055556052338848388, 4.084588180558401227, -2.925285743277528550 ) ) ;
#14347 = AXIS2_PLACEMENT_3D ( 'NONE', #37, #3678, #8239 ) ;
#14348 = AXIS2_PLACEMENT_3D ( 'NONE', #14124, #7556, #10798 ) ;
#14349 = CIRCLE ( 'NONE', #8412, 0.1000000000000002554 ) ;
#14350 = EDGE_CURVE ( 'NONE', #1573, #4609, #1180, .T. ) ;
#14351 = LINE ( 'NONE', #8955, #3331 ) ;
#14352 = B_SPLINE_CURVE_WITH_KNOTS ( 'NONE', 3,
 ( #3674, #3899, #2642, #10524 ),
 .UNSPECIFIED., .F., .F.,
 ( 4, 4 ),
 ( 2.380735200829041677E-07, 0.002921158011986708155 ),
 .UNSPECIFIED. ) ;
#14353 = ADVANCED_FACE ( 'NONE', ( #5119 ), #14390, .T. ) ;
#14354 = ORIENTED_EDGE ( 'NONE', *, *, #8786, .F. ) ;
#14355 = ORIENTED_EDGE ( 'NONE', *, *, #10760, .F. ) ;
#14356 = CARTESIAN_POINT ( 'NONE',  ( 153.1991633467111456, 386.6211705227183870, -190.0000000000000000 ) ) ;
#14357 = CARTESIAN_POINT ( 'NONE',  ( 6.818262094730843437, 1.323628772216571381, -6.207787212118422104 ) ) ;
#14358 = AXIS2_PLACEMENT_3D ( 'NONE', #6888, #3490, #10132 ) ;
#14359 = VECTOR ( 'NONE', #14473, 1000.000000000000114 ) ;
#14360 = CARTESIAN_POINT ( 'NONE',  ( 4.000000000000000000, 2.309401076758497151, -3.433295621305379353 ) ) ;
#14361 = LINE ( 'NONE', #5354, #9962 ) ;
#14362 = ORIENTED_EDGE ( 'NONE', *, *, #1586, .F. ) ;
#14363 = CARTESIAN_POINT ( 'NONE',  ( 639.0000000000000000, 156.0000000000000000, -225.5000000000000000 ) ) ;
#14364 = ORIENTED_EDGE ( 'NONE', *, *, #9307, .F. ) ;
#14365 = DIRECTION ( 'NONE',  ( 0.000000000000000000, 0.000000000000000000, -1.000000000000000000 ) ) ;
#14366 = AXIS2_PLACEMENT_3D ( 'NONE', #7814, #12087, #9955 ) ;
#14367 = ORIENTED_EDGE ( 'NONE', *, *, #14132, .T. ) ;
#14368 = AXIS2_PLACEMENT_3D ( 'NONE', #1266, #2664, #10416 ) ;
#14369 = AXIS2_PLACEMENT_3D ( 'NONE', #5154, #10914, #9660 ) ;
#14370 = CARTESIAN_POINT ( 'NONE',  ( 2.000000000000000000, -6.429618962271402616, 0.000000000000000000 ) ) ;
#14371 = DIRECTION ( 'NONE',  ( -1.000000000000000000, -0.000000000000000000, -0.000000000000000000 ) ) ;
#14372 = ORIENTED_EDGE ( 'NONE', *, *, #12305, .T. ) ;
#14373 = CARTESIAN_POINT ( 'NONE',  ( 610.2394425817745969, 189.6441153868865399, 186.5350371479513569 ) ) ;
#14374 = CARTESIAN_POINT ( 'NONE',  ( 33.05499999999999972, 0.000000000000000000, 2.500000000000000444 ) ) ;
#14375 = VECTOR ( 'NONE', #4275, 1000.000000000000114 ) ;
#14376 = DIRECTION ( 'NONE',  ( -0.9578262852211518741, 0.2873478855663437748, 0.000000000000000000 ) ) ;
#14377 = EDGE_LOOP ( 'NONE', ( #3653, #5029, #13747, #327 ) ) ;
#14378 = AXIS2_PLACEMENT_3D ( 'NONE', #10984, #11273, #10096 ) ;
#14379 = CIRCLE ( 'NONE', #2601, 2.100000000000000089 ) ;
#14380 = CARTESIAN_POINT ( 'NONE',  ( 723.3240306373314752, 157.9460551874147427, -149.9999999999986358 ) ) ;
#14381 = ORIENTED_EDGE ( 'NONE', *, *, #7592, .T. ) ;
#14382 = EDGE_CURVE ( 'NONE', #7674, #8837, #8733, .T. ) ;
#14383 = EDGE_LOOP ( 'NONE', ( #2486, #14461 ) ) ;
#14385 = FACE_OUTER_BOUND ( 'NONE', #7530, .T. ) ;
#14384 = AXIS2_PLACEMENT_3D ( 'NONE', #7539, #4300, #5182 ) ;
#14386 = VECTOR ( 'NONE', #13670, 1000.000000000000000 ) ;
#14387 = CARTESIAN_POINT ( 'NONE',  ( 7.240873133980792353, 470.9098836221797342, 190.0000000000001990 ) ) ;
#14389 = AXIS2_PLACEMENT_3D ( 'NONE', #4849, #11258, #3665 ) ;
#14388 = CARTESIAN_POINT ( 'NONE',  ( 8.500000000000000000, 0.000000000000000000, 0.000000000000000000 ) ) ;
#14390 = CONICAL_SURFACE ( 'NONE', #4261, 5.000000000000000888, 1.047197551196600296 ) ;
#14391 = CARTESIAN_POINT ( 'NONE',  ( 4.000000000000000000, 0.000000000000000000, 0.000000000000000000 ) ) ;
#14392 = VECTOR ( 'NONE', #7450, 1000.000000000000000 ) ;
#14393 = DIRECTION ( 'NONE',  ( -0.000000000000000000, 0.8660254037844391517, 0.4999999999999990563 ) ) ;
#14394 = ORIENTED_EDGE ( 'NONE', *, *, #2775, .F. ) ;
#14395 = AXIS2_PLACEMENT_3D ( 'NONE', #12321, #9078, #11215 ) ;
#14396 = CARTESIAN_POINT ( 'NONE',  ( 627.2408731339806991, 284.9098836221800184, -190.0000000000001990 ) ) ;
#14397 = CARTESIAN_POINT ( 'NONE',  ( 8.542937654374687995, 1.046208125374536008E-15, -6.800000000000000711 ) ) ;
#14398 = APPLICATION_PROTOCOL_DEFINITION ( 'draft international standard', 'automotive_design', 1998, #5288 ) ;
#14399 = ADVANCED_FACE ( 'NONE', ( #1787 ), #9207, .T. ) ;
#14400 = CIRCLE ( 'NONE', #8985, 0.6186547224754559426 ) ;
#14401 = DIRECTION ( 'NONE',  ( 0.9578262852211517631, -0.2873478855663438858, 0.000000000000000000 ) ) ;
#14402 = ORIENTED_EDGE ( 'NONE', *, *, #2310, .T. ) ;
#14403 = EDGE_LOOP ( 'NONE', ( #13937, #6197, #13631, #8861, #6467 ) ) ;
#14404 = SURFACE_STYLE_USAGE ( .BOTH. , #13357 ) ;
#14405 = CARTESIAN_POINT ( 'NONE',  ( 610.0000000000001137, 185.6790804732684421, -187.0000000000000000 ) ) ;
#14406 = EDGE_CURVE ( 'NONE', #358, #6378, #4243, .T. ) ;
#14407 = CARTESIAN_POINT ( 'NONE',  ( -1.269541193505925744E-15, 7.895640089090863789, -6.564402953523717166 ) ) ;
#14408 = AXIS2_PLACEMENT_3D ( 'NONE', #2323, #1144, #3604 ) ;
#14409 = AXIS2_PLACEMENT_3D ( 'NONE', #3734, #10510, #378 ) ;
#14410 = ADVANCED_FACE ( 'NONE', ( #6992 ), #3621, .T. ) ;
#14411 = PRODUCT_DEFINITION_SHAPE ( 'NONE', 'NONE',  #4059 ) ;
#14412 = LINE ( 'NONE', #6662, #7792 ) ;
#14413 = VECTOR ( 'NONE', #1813, 1000.000000000000000 ) ;
#14414 = ORIENTED_EDGE ( 'NONE', *, *, #3686, .T. ) ;
#14415 = ADVANCED_FACE ( 'NONE', ( #10401, #13642 ), #7958, .T. ) ;
#14416 = MECHANICAL_DESIGN_GEOMETRIC_PRESENTATION_REPRESENTATION (  '', ( #11810 ), #1684 ) ;
#14417 = CARTESIAN_POINT ( 'NONE',  ( 628.0000000000000000, 242.0000000000000568, -233.5000000000000000 ) ) ;
#14418 = ORIENTED_EDGE ( 'NONE', *, *, #5456, .T. ) ;
#14419 = CARTESIAN_POINT ( 'NONE',  ( 604.3113219698374223, -181.2933965909545293, 9.397040286797935582E-13 ) ) ;
#14420 = FACE_OUTER_BOUND ( 'NONE', #4380, .T. ) ;
#14421 = LINE ( 'NONE', #4313, #12933 ) ;
#14422 = AXIS2_PLACEMENT_3D ( 'NONE', #9998, #7787, #4388 ) ;
#14423 = ORIENTED_EDGE ( 'NONE', *, *, #5240, .T. ) ;
#14424 = DIRECTION ( 'NONE',  ( 0.000000000000000000, 0.000000000000000000, -1.000000000000000000 ) ) ;
#14425 = ORIENTED_EDGE ( 'NONE', *, *, #14432, .F. ) ;
#14426 = ORIENTED_EDGE ( 'NONE', *, *, #3396, .F. ) ;
#14427 = DIRECTION ( 'NONE',  ( -1.000000000000000000, 0.000000000000000000, 0.000000000000000000 ) ) ;
#14428 = APPLICATION_CONTEXT ( 'automotive_design' ) ;
#14429 = STYLED_ITEM ( 'NONE', ( #14274 ), #7024 ) ;
#14430 = SHAPE_REPRESENTATION ( 'sliding track', ( #9440 ), #1445 ) ;
#14431 = CARTESIAN_POINT ( 'NONE',  ( 4.000000000000000000, 2.309401076758497151, -3.433295621305379353 ) ) ;
#14432 = EDGE_CURVE ( 'NONE', #3740, #10150, #13508, .T. ) ;
#14433 = EDGE_CURVE ( 'NONE', #7000, #11781, #8106, .T. ) ;
#14434 = CARTESIAN_POINT ( 'NONE',  ( 0.2500000000000002220, 4.898587196589412829E-16, -4.000000000000000000 ) ) ;
#14435 = AXIS2_PLACEMENT_3D ( 'NONE', #943, #12313, #1087 ) ;
#14436 = ORIENTED_EDGE ( 'NONE', *, *, #10433, .T. ) ;
#14437 = EDGE_CURVE ( 'NONE', #8674, #9517, #12381, .T. ) ;
#14438 = ORIENTED_EDGE ( 'NONE', *, *, #12669, .T. ) ;
#14439 = FACE_BOUND ( 'NONE', #11488, .T. ) ;
#14440 = CARTESIAN_POINT ( 'NONE',  ( 6.499999999999999112, 4.014041399406598210, -6.470356572124273953 ) ) ;
#14441 = ORIENTED_EDGE ( 'NONE', *, *, #10616, .T. ) ;
#14442 = CARTESIAN_POINT ( 'NONE',  ( 641.0000000000000000, 154.0000000000000568, 187.5000000000000000 ) ) ;
#14443 = CYLINDRICAL_SURFACE ( 'NONE', #2056, 2.649999999999985700 ) ;
#14444 = DIRECTION ( 'NONE',  ( 1.000000000000000000, 0.000000000000000000, 0.000000000000000000 ) ) ;
#14445 = ORIENTED_EDGE ( 'NONE', *, *, #6645, .F. ) ;
#14446 = FILL_AREA_STYLE ('',( #5295 ) ) ;
#14447 = ORIENTED_EDGE ( 'NONE', *, *, #4923, .T. ) ;
#14448 = FACE_OUTER_BOUND ( 'NONE', #6254, .T. ) ;
#14449 = VERTEX_POINT ( 'NONE', #1166 ) ;
#14450 = PRODUCT_DEFINITION_SHAPE ( 'NONE', 'NONE',  #14646 ) ;
#14451 = DIRECTION ( 'NONE',  ( 1.000000000000000000, 0.000000000000000000, -0.000000000000000000 ) ) ;
#14452 = FACE_OUTER_BOUND ( 'NONE', #7194, .T. ) ;
#14453 = AXIS2_PLACEMENT_3D ( 'NONE', #6701, #13626, #12368 ) ;
#14454 = ORIENTED_EDGE ( 'NONE', *, *, #8988, .T. ) ;
#14455 = CARTESIAN_POINT ( 'NONE',  ( 2.345747346278113987, -3.264484291692503870, -0.01223254789874484924 ) ) ;
#14456 = DIRECTION ( 'NONE',  ( -1.000000000000000000, 0.000000000000000000, -0.000000000000000000 ) ) ;
#14457 = DIRECTION ( 'NONE',  ( 0.9578262852211525402, -0.2873478855663419429, -0.000000000000000000 ) ) ;
#14458 = ORIENTED_EDGE ( 'NONE', *, *, #4871, .T. ) ;
#14459 =( NAMED_UNIT ( * ) SI_UNIT ( $, .STERADIAN. ) SOLID_ANGLE_UNIT ( ) );
#14460 = ORIENTED_EDGE ( 'NONE', *, *, #10146, .F. ) ;
#14461 = ORIENTED_EDGE ( 'NONE', *, *, #2595, .T. ) ;
#14462 = DIRECTION ( 'NONE',  ( 1.000000000000000000, 0.000000000000000000, 0.000000000000000000 ) ) ;
#14463 = CLOSED_SHELL ( 'NONE', ( #4654, #7850, #7740, #10853, #2068, #9813, #9727, #13012, #12873, #1040, #5473, #13960, #1837, #6882, #10535, #12567, #13776, #5715, #6211, #10445, #6274, #12168 ) ) ;
#14464 = CARTESIAN_POINT ( 'NONE',  ( 627.5000000000000000, 160.0000000000000284, -225.5000000000000000 ) ) ;
#14465 = DIRECTION ( 'NONE',  ( -0.2873478855663453846, -0.9578262852211513190, -0.000000000000000000 ) ) ;
#14466 = EDGE_CURVE ( 'NONE', #6264, #483, #5750, .T. ) ;
#14467 = DIRECTION ( 'NONE',  ( -1.000000000000000000, -0.000000000000000000, -0.000000000000000000 ) ) ;
#14468 = CARTESIAN_POINT ( 'NONE',  ( 4.000000000000000000, 0.1981133338132474442, 2.382280164152719704E-17 ) ) ;
#14469 = CARTESIAN_POINT ( 'NONE',  ( -6.818272094961329799, -1.321852500971156363, -6.208027553811807486 ) ) ;
#14470 = VERTEX_POINT ( 'NONE', #4506 ) ;
#14471 = PRODUCT_DEFINITION_CONTEXT ( 'detailed design', #4340, 'design' ) ;
#14472 = CARTESIAN_POINT ( 'NONE',  ( -3.399999999999999911, 4.163799117101000559E-16, -0.4201245229258211977 ) ) ;
#14473 = DIRECTION ( 'NONE',  ( -0.2873478855663418874, -0.9578262852211524292, -1.261617073437818631E-13 ) ) ;
#14474 = PRODUCT_CONTEXT ( 'NONE', #7062, 'mechanical' ) ;
#14475 = CARTESIAN_POINT ( 'NONE',  ( -12.99999999999999112, -3.903127820947815962E-15, -8.000000000000000000 ) ) ;
#14476 = ORIENTED_EDGE ( 'NONE', *, *, #2803, .T. ) ;
#14477 = ORIENTED_EDGE ( 'NONE', *, *, #1726, .T. ) ;
#14478 = SURFACE_STYLE_FILL_AREA ( #11151 ) ;
#14479 = CYLINDRICAL_SURFACE ( 'NONE', #9018, 6.750000000000000000 ) ;
#14480 = DIRECTION ( 'NONE',  ( 0.000000000000000000, 0.000000000000000000, 1.000000000000000000 ) ) ;
#14481 = EDGE_CURVE ( 'NONE', #11591, #1324, #6856, .T. ) ;
#14482 = CARTESIAN_POINT ( 'NONE',  ( 6.244297270354684848, -1.799661607120071246E-11, -5.105276777067894400 ) ) ;
#14483 = VERTEX_POINT ( 'NONE', #6711 ) ;
#14484 = CARTESIAN_POINT ( 'NONE',  ( -6.838249472399978046, -3.995156693690920413, -6.573189567101943354 ) ) ;
#14485 = EDGE_LOOP ( 'NONE', ( #893, #6310, #12762, #876 ) ) ;
#14486 = DIRECTION ( 'NONE',  ( -1.000000000000000000, -0.000000000000000000, -0.000000000000000000 ) ) ;
#14487 = CARTESIAN_POINT ( 'NONE',  ( 635.0000000000000000, 160.0000000000000284, 210.0000000000000000 ) ) ;
#14488 = CARTESIAN_POINT ( 'NONE',  ( 702.5260191523638014, 164.1854586329053518, 177.6000000000001648 ) ) ;
#14489 = APPLICATION_PROTOCOL_DEFINITION ( 'draft international standard', 'automotive_design', 1998, #12826 ) ;
#14490 = ADVANCED_FACE ( 'NONE', ( #4731 ), #4502, .T. ) ;
#14491 = DIRECTION ( 'NONE',  ( 0.000000000000000000, 0.000000000000000000, 1.000000000000000000 ) ) ;
#14492 = ORIENTED_EDGE ( 'NONE', *, *, #11960, .T. ) ;
#14493 = ORIENTED_EDGE ( 'NONE', *, *, #13339, .T. ) ;
#14494 = CARTESIAN_POINT ( 'NONE',  ( -0.6666666666666651864, 4.233901974057260098, -3.300726591567081147 ) ) ;
#14495 = DIRECTION ( 'NONE',  ( -1.000000000000000000, -0.000000000000000000, -0.000000000000000000 ) ) ;
#14496 = DIRECTION ( 'NONE',  ( 0.000000000000000000, 0.000000000000000000, 1.000000000000000000 ) ) ;
#14497 = EDGE_CURVE ( 'NONE', #2298, #4638, #5440, .T. ) ;
#14498 = ORIENTED_EDGE ( 'NONE', *, *, #6024, .F. ) ;
#14499 = VERTEX_POINT ( 'NONE', #5600 ) ;
#14500 = LINE ( 'NONE', #12273, #11357 ) ;
#14501 = DIRECTION ( 'NONE',  ( 0.000000000000000000, 0.000000000000000000, 1.000000000000000000 ) ) ;
#14502 = CYLINDRICAL_SURFACE ( 'NONE', #4203, 4.199999999999926459 ) ;
#14503 = CARTESIAN_POINT ( 'NONE',  ( 630.5661054975340676, 158.1613647612965110, 211.0000000000000000 ) ) ;
#14504 = CARTESIAN_POINT ( 'NONE',  ( 139.8040310085880833, 355.9707293956415697, 190.0000000000000000 ) ) ;
#14505 = SHAPE_REPRESENTATION_RELATIONSHIP ( 'NONE' , 'NONE' ,  #3781, #11776 ) ;
#14506 = EDGE_LOOP ( 'NONE', ( #6719, #1978, #1846, #12270, #10215 ) ) ;
#14507 = ADVANCED_FACE ( 'NONE', ( #5680, #10102 ), #9002, .T. ) ;
#14508 = SURFACE_STYLE_USAGE ( .BOTH. , #10004 ) ;
#14509 = ITEM_DEFINED_TRANSFORMATION ( 'NONE', 'NONE', #11132,  #9440 ) ;
#14510 = VERTEX_POINT ( 'NONE', #1385 ) ;
#14511 = ORIENTED_EDGE ( 'NONE', *, *, #4803, .T. ) ;
#14512 = CARTESIAN_POINT ( 'NONE',  ( 2.999999999999999112, 4.000000000000000000, 0.000000000000000000 ) ) ;
#14513 = ADVANCED_FACE ( 'NONE', ( #10318 ), #2491, .F. ) ;
#14514 = VERTEX_POINT ( 'NONE', #9220 ) ;
#14515 = PRODUCT_DEFINITION ( 'UNKNOWN', '', #12078, #14034 ) ;
#14516 = CARTESIAN_POINT ( 'NONE',  ( 708.1388811837593948, 164.7984674554458593, -182.7999999999999261 ) ) ;
#14517 = DIRECTION ( 'NONE',  ( -0.000000000000000000, -0.000000000000000000, 1.000000000000000000 ) ) ;
#14518 = VERTEX_POINT ( 'NONE', #13729 ) ;
#14519 = CARTESIAN_POINT ( 'NONE',  ( 0.4465819873851997746, 2.886751345948125547, 4.999999999999999112 ) ) ;
#14520 = DIRECTION ( 'NONE',  ( 0.000000000000000000, 0.000000000000000000, 1.000000000000000000 ) ) ;
#14521 = FACE_OUTER_BOUND ( 'NONE', #14068, .T. ) ;
#14522 = SURFACE_STYLE_USAGE ( .BOTH. , #13195 ) ;
#14523 = ORIENTED_EDGE ( 'NONE', *, *, #5928, .T. ) ;
#14524 = VERTEX_POINT ( 'NONE', #10249 ) ;
#14525 = ORIENTED_EDGE ( 'NONE', *, *, #6101, .F. ) ;
#14526 = CYLINDRICAL_SURFACE ( 'NONE', #3983, 20.00000000000001776 ) ;
#14527 = DIRECTION ( 'NONE',  ( 0.000000000000000000, 0.000000000000000000, 1.000000000000000000 ) ) ;
#14528 = CARTESIAN_POINT ( 'NONE',  ( 638.7884810776471340, 166.5485936625643717, -210.0000000000000000 ) ) ;
#14529 = ADVANCED_FACE ( 'NONE', ( #11492 ), #2431, .T. ) ;
#14530 = DIRECTION ( 'NONE',  ( -1.000000000000000000, 0.000000000000000000, 0.000000000000000000 ) ) ;
#14531 = EDGE_CURVE ( 'NONE', #12815, #8086, #9529, .T. ) ;
#14532 = DIRECTION ( 'NONE',  ( -0.9578262852211507639, 0.2873478855663477716, 0.000000000000000000 ) ) ;
#14533 = CARTESIAN_POINT ( 'NONE',  ( 2.500000000000000000, 1.178949249685212974, -2.042000000000001148 ) ) ;
#14534 = DIRECTION ( 'NONE',  ( 0.000000000000000000, 0.000000000000000000, -1.000000000000000000 ) ) ;
#14535 = ORIENTED_EDGE ( 'NONE', *, *, #7954, .T. ) ;
#14536 = CARTESIAN_POINT ( 'NONE',  ( 631.0000000000000000, 155.9999999999999432, -233.5000000000000000 ) ) ;
#14537 = CARTESIAN_POINT ( 'NONE',  ( 6.534838248920900483, -5.903531555104837736, 5.201568163584232486E-16 ) ) ;
#14538 = SHAPE_DEFINITION_REPRESENTATION ( #7608, #6959 ) ;
#14539 = DIRECTION ( 'NONE',  ( 0.000000000000000000, 0.000000000000000000, 1.000000000000000000 ) ) ;
#14540 = EDGE_LOOP ( 'NONE', ( #13553, #10252, #1945, #7874, #13650, #3512, #8599 ) ) ;
#14541 = ORIENTED_EDGE ( 'NONE', *, *, #12109, .F. ) ;
#14542 =( NAMED_UNIT ( * ) PLANE_ANGLE_UNIT ( ) SI_UNIT ( $, .RADIAN. ) );
#14543 = FACE_OUTER_BOUND ( 'NONE', #14038, .T. ) ;
#14544 = ADVANCED_FACE ( 'NONE', ( #1473 ), #11317, .T. ) ;
#14546 = CARTESIAN_POINT ( 'NONE',  ( 2.500000000000000000, 2.357898499370431722, -2.818925648462311528E-15 ) ) ;
#14545 = AXIS2_PLACEMENT_3D ( 'NONE', #2543, #1449, #163 ) ;
#14547 = CARTESIAN_POINT ( 'NONE',  ( -5.589124336234651658, 4.278671059406048194, -6.219623095967983240 ) ) ;
#14548 = ORIENTED_EDGE ( 'NONE', *, *, #5847, .T. ) ;
#14549 = CARTESIAN_POINT ( 'NONE',  ( 590.0000000000000000, -9.999999999999944933, 190.0000000000000000 ) ) ;
#14550 = EDGE_LOOP ( 'NONE', ( #14436, #11632 ) ) ;
#14551 = COLOUR_RGB ( '',1.000000000000000000, 0.9490196078431372140, 0.9098039215686274384 ) ;
#14552 = AXIS2_PLACEMENT_3D ( 'NONE', #1506, #458, #7117 ) ;
#14553 = CYLINDRICAL_SURFACE ( 'NONE', #8688, 2.649999999999985700 ) ;
#14554 = FACE_OUTER_BOUND ( 'NONE', #3839, .T. ) ;
#14555 =( NAMED_UNIT ( * ) PLANE_ANGLE_UNIT ( ) SI_UNIT ( $, .RADIAN. ) );
#14556 = AXIS2_PLACEMENT_3D ( 'NONE', #8267, #7090, #516 ) ;
#14557 = LINE ( 'NONE', #12477, #5444 ) ;
#14558 = ORIENTED_EDGE ( 'NONE', *, *, #3217, .F. ) ;
#14559 = VERTEX_POINT ( 'NONE', #1690 ) ;
#14560 = DIRECTION ( 'NONE',  ( 1.000000000000000000, 0.000000000000000000, 0.000000000000000000 ) ) ;
#14561 = EDGE_CURVE ( 'NONE', #7721, #11030, #12982, .T. ) ;
#14562 = CARTESIAN_POINT ( 'NONE',  ( 4.000000000000000000, 2.309401076758497151, -5.000000000000000000 ) ) ;
#14563 = AXIS2_PLACEMENT_3D ( 'NONE', #6279, #659, #11950 ) ;
#14564 = CARTESIAN_POINT ( 'NONE',  ( -20.63749999999999574, 8.266365894244634333E-16, 6.750000000000000000 ) ) ;
#14565 = VECTOR ( 'NONE', #2267, 1000.000000000000000 ) ;
#14566 = EDGE_LOOP ( 'NONE', ( #5510, #11702, #14477, #6299 ) ) ;
#14567 = ORIENTED_EDGE ( 'NONE', *, *, #6463, .T. ) ;
#14568 = CARTESIAN_POINT ( 'NONE',  ( 609.9913795634330427, 185.6503456847118514, -184.8000000000000966 ) ) ;
#14569 = CARTESIAN_POINT ( 'NONE',  ( 107.2182642636026202, 357.3942142120087055, 210.0000000000000000 ) ) ;
#14570 = PLANE ( 'NONE',  #8182 ) ;
#14571 = DIRECTION ( 'NONE',  ( 1.000000000000000000, 0.000000000000000000, 0.000000000000000000 ) ) ;
#14572 = EDGE_LOOP ( 'NONE', ( #11551, #9045, #6649, #6903 ) ) ;
#14573 = VECTOR ( 'NONE', #7082, 1000.000000000000000 ) ;
#14574 = DIRECTION ( 'NONE',  ( 0.000000000000000000, 0.000000000000000000, -1.000000000000000000 ) ) ;
#14575 = AXIS2_PLACEMENT_3D ( 'NONE', #9387, #210, #13749 ) ;
#14576 = AXIS2_PLACEMENT_3D ( 'NONE', #8963, #7789, #9933 ) ;
#14577 = VERTEX_POINT ( 'NONE', #1754 ) ;
#14578 = EDGE_LOOP ( 'NONE', ( #7695, #3404, #8537, #8315 ) ) ;
#14579 = CARTESIAN_POINT ( 'NONE',  ( 635.0000000000000000, 160.0000000000000284, -211.0000000000000000 ) ) ;
#14580 = EDGE_CURVE ( 'NONE', #3847, #611, #10618, .T. ) ;
#14581 = EDGE_LOOP ( 'NONE', ( #5832, #2084, #6635, #9974 ) ) ;
#14582 = EDGE_CURVE ( 'NONE', #2514, #4781, #11784, .T. ) ;
#14583 = CARTESIAN_POINT ( 'NONE',  ( 0.1739375980333479899, -3.358985280702904586, -4.182066831946573693 ) ) ;
#14584 = EDGE_CURVE ( 'NONE', #4991, #12841, #9663, .T. ) ;
#14585 = LINE ( 'NONE', #12292, #13001 ) ;
#14586 = VECTOR ( 'NONE', #2383, 1000.000000000000000 ) ;
#14587 = EDGE_CURVE ( 'NONE', #12715, #3037, #7371, .T. ) ;
#14588 = AXIS2_PLACEMENT_3D ( 'NONE', #6214, #10932, #8572 ) ;
#14589 = ORIENTED_EDGE ( 'NONE', *, *, #7012, .T. ) ;
#14590 = LINE ( 'NONE', #8014, #4298 ) ;
#14591 = CARTESIAN_POINT ( 'NONE',  ( 707.5067158355136598, 162.6912496279593938, -177.6000000000005059 ) ) ;
#14592 = ADVANCED_FACE ( 'NONE', ( #2569 ), #11641, .F. ) ;
#14593 =( BOUNDED_SURFACE ( )  B_SPLINE_SURFACE ( 3, 2, ( 
 ( #14268, #8650, #4307 ),
 ( #12041, #12177, #1939 ),
 ( #817, #5334, #8804 ),
 ( #14337, #4229, #8730 ),
 ( #2066, #13300, #3193 ),
 ( #6585, #11083, #14484 ) ),
 .UNSPECIFIED., .F., .F., .T. ) 
 B_SPLINE_SURFACE_WITH_KNOTS ( ( 4, 2, 4 ),
 ( 3, 3 ),
 ( 0.03172058138205611361, 0.03571597378202086281, 0.03971136618198560508 ),
 ( 0.000000000000000000, 1.000000000000000000 ),
 .UNSPECIFIED. ) 
 GEOMETRIC_REPRESENTATION_ITEM ( )  RATIONAL_B_SPLINE_SURFACE ( (
 ( 1.000000000000000000, 0.8047780791350982454, 1.000000000000000000),
 ( 1.000000000000000000, 0.8123796029720318224, 1.000000000000000000),
 ( 1.000000000000000000, 0.8190681660673523323, 1.000000000000000000),
 ( 1.000000000000000000, 0.8192342536572917444, 1.000000000000000000),
 ( 1.000000000000000000, 0.8126124427164184150, 1.000000000000000000),
 ( 1.000000000000000000, 0.8047712715942066941, 1.000000000000000000) ) ) 
 REPRESENTATION_ITEM ( '' )  SURFACE ( )  );
#14594 = CARTESIAN_POINT ( 'NONE',  ( -8.505790995054828940, 418.4210031920615620, -184.7999999999999829 ) ) ;
#14595 = PLANE ( 'NONE',  #14453 ) ;
#14596 = SURFACE_STYLE_FILL_AREA ( #10088 ) ;
#14597 = ORIENTED_EDGE ( 'NONE', *, *, #1765, .F. ) ;
#14598 = DIRECTION ( 'NONE',  ( 0.9578262852211513190, -0.2873478855663455511, -5.916456789157588541E-31 ) ) ;
#14599 = ORIENTED_EDGE ( 'NONE', *, *, #14582, .F. ) ;
#14600 = AXIS2_PLACEMENT_3D ( 'NONE', #4818, #4959, #10332 ) ;
#14601 = CIRCLE ( 'NONE', #9417, 6.975000000000000533 ) ;
#14602 = ORIENTED_EDGE ( 'NONE', *, *, #2307, .T. ) ;
#14603 = FACE_OUTER_BOUND ( 'NONE', #2656, .T. ) ;
#14604 = CYLINDRICAL_SURFACE ( 'NONE', #11545, 7.500000000000000000 ) ;
#14606 = EDGE_CURVE ( 'NONE', #1758, #808, #3977, .T. ) ;
#14605 = AXIS2_PLACEMENT_3D ( 'NONE', #32, #10091, #4570 ) ;
#14607 = CARTESIAN_POINT ( 'NONE',  ( 6.500000000000000000, -0.6456425506958747285, 7.487771253728014997E-16 ) ) ;
#14608 = EDGE_CURVE ( 'NONE', #5340, #10297, #13233, .T. ) ;
#14609 = PLANE ( 'NONE',  #501 ) ;
#14610 = VECTOR ( 'NONE', #626, 1000.000000000000114 ) ;
#14611 = VECTOR ( 'NONE', #8444, 1000.000000000000000 ) ;
#14612 = CARTESIAN_POINT ( 'NONE',  ( 0.000000000000000000, -3.464101615137757051, -1.999999999999996225 ) ) ;
#14613 = CARTESIAN_POINT ( 'NONE',  ( 0.000000000000000000, 0.000000000000000000, -4.000000000000000000 ) ) ;
#14614 = CYLINDRICAL_SURFACE ( 'NONE', #12597, 4.199999999999981526 ) ;
#14615 = APPLICATION_CONTEXT ( 'automotive_design' ) ;
#14616 = CARTESIAN_POINT ( 'NONE',  ( 459.7035746174795463, 294.6698471414878782, 190.0000000000000000 ) ) ;
#14617 = NEXT_ASSEMBLY_USAGE_OCCURRENCE ( 'NAUO1', ' ', ' ', #11257, #6844, $ ) ;
#14618 = NEXT_ASSEMBLY_USAGE_OCCURRENCE ( 'NAUO2', ' ', ' ', #11257, #5588, $ ) ;
#14619 = NEXT_ASSEMBLY_USAGE_OCCURRENCE ( 'NAUO3', ' ', ' ', #11257, #13442, $ ) ;
#14620 = NEXT_ASSEMBLY_USAGE_OCCURRENCE ( 'NAUO4', ' ', ' ', #11257, #14515, $ ) ;
#14621 = NEXT_ASSEMBLY_USAGE_OCCURRENCE ( 'NAUO5', ' ', ' ', #11257, #8184, $ ) ;
#14622 = NEXT_ASSEMBLY_USAGE_OCCURRENCE ( 'NAUO6', ' ', ' ', #11257, #5765, $ ) ;
#14623 = NEXT_ASSEMBLY_USAGE_OCCURRENCE ( 'NAUO7', ' ', ' ', #11257, #9740, $ ) ;
#14624 = NEXT_ASSEMBLY_USAGE_OCCURRENCE ( 'NAUO8', ' ', ' ', #11257, #8642, $ ) ;
#14625 = NEXT_ASSEMBLY_USAGE_OCCURRENCE ( 'NAUO9', ' ', ' ', #11257, #1603, $ ) ;
#14626 = NEXT_ASSEMBLY_USAGE_OCCURRENCE ( 'NAUO10', ' ', ' ', #11257, #13881, $ ) ;
#14627 = NEXT_ASSEMBLY_USAGE_OCCURRENCE ( 'NAUO11', ' ', ' ', #11257, #13881, $ ) ;
#14628 = NEXT_ASSEMBLY_USAGE_OCCURRENCE ( 'NAUO12', ' ', ' ', #11257, #1603, $ ) ;
#14629 = NEXT_ASSEMBLY_USAGE_OCCURRENCE ( 'NAUO13', ' ', ' ', #11257, #9297, $ ) ;
#14630 = NEXT_ASSEMBLY_USAGE_OCCURRENCE ( 'NAUO14', ' ', ' ', #11257, #972, $ ) ;
#14631 = NEXT_ASSEMBLY_USAGE_OCCURRENCE ( 'NAUO15', ' ', ' ', #11257, #12337, $ ) ;
#14632 = NEXT_ASSEMBLY_USAGE_OCCURRENCE ( 'NAUO16', ' ', ' ', #11257, #12337, $ ) ;
#14633 = NEXT_ASSEMBLY_USAGE_OCCURRENCE ( 'NAUO17', ' ', ' ', #11257, #10810, $ ) ;
#14634 = NEXT_ASSEMBLY_USAGE_OCCURRENCE ( 'NAUO18', ' ', ' ', #11257, #10810, $ ) ;
#14635 = NEXT_ASSEMBLY_USAGE_OCCURRENCE ( 'NAUO19', ' ', ' ', #11257, #4059, $ ) ;
#14636 = NEXT_ASSEMBLY_USAGE_OCCURRENCE ( 'NAUO20', ' ', ' ', #11257, #4059, $ ) ;
#14637 = NEXT_ASSEMBLY_USAGE_OCCURRENCE ( 'NAUO21', ' ', ' ', #11257, #8374, $ ) ;
#14638 = NEXT_ASSEMBLY_USAGE_OCCURRENCE ( 'NAUO22', ' ', ' ', #11257, #8374, $ ) ;
#14639 = NEXT_ASSEMBLY_USAGE_OCCURRENCE ( 'NAUO23', ' ', ' ', #11257, #8374, $ ) ;
#14640 = NEXT_ASSEMBLY_USAGE_OCCURRENCE ( 'NAUO24', ' ', ' ', #11257, #4059, $ ) ;
#14641 = NEXT_ASSEMBLY_USAGE_OCCURRENCE ( 'NAUO25', ' ', ' ', #11257, #10810, $ ) ;
#14642 = NEXT_ASSEMBLY_USAGE_OCCURRENCE ( 'NAUO26', ' ', ' ', #11257, #12337, $ ) ;
#14643 = NEXT_ASSEMBLY_USAGE_OCCURRENCE ( 'NAUO27', ' ', ' ', #11257, #8374, $ ) ;
#14644 = NEXT_ASSEMBLY_USAGE_OCCURRENCE ( 'NAUO28', ' ', ' ', #11257, #4059, $ ) ;
#14645 = NEXT_ASSEMBLY_USAGE_OCCURRENCE ( 'NAUO29', ' ', ' ', #11257, #10810, $ ) ;
#14646 = NEXT_ASSEMBLY_USAGE_OCCURRENCE ( 'NAUO30', ' ', ' ', #11257, #12337, $ ) ;
#14647=COLOUR_RGB('Dark Blue',0.08,0.2,0.34);
#14648=FILL_AREA_STYLE_COLOUR('',#14647);
#14649=FILL_AREA_STYLE('',(#14648));
#14650=SURFACE_STYLE_FILL_AREA(#14649);
#14651=SURFACE_SIDE_STYLE('',(#14650));
#14652=SURFACE_STYLE_USAGE(.BOTH.,#14651);
#14653=PRESENTATION_STYLE_ASSIGNMENT((#14652));
#14654=COLOUR_RGB('Light Blue',0.38,0.62,0.78);
#14655=FILL_AREA_STYLE_COLOUR('',#14654);
#14656=FILL_AREA_STYLE('',(#14655));
#14657=SURFACE_STYLE_FILL_AREA(#14656);
#14658=SURFACE_SIDE_STYLE('',(#14657));
#14659=SURFACE_STYLE_USAGE(.BOTH.,#14658);
#14660=PRESENTATION_STYLE_ASSIGNMENT((#14659));
#14661=COLOUR_RGB('Sky Blue',0.24,0.69,0.87);
#14662=FILL_AREA_STYLE_COLOUR('',#14661);
#14663=FILL_AREA_STYLE('',(#14662));
#14664=SURFACE_STYLE_FILL_AREA(#14663);
#14665=SURFACE_SIDE_STYLE('',(#14664));
#14666=SURFACE_STYLE_USAGE(.BOTH.,#14665);
#14667=PRESENTATION_STYLE_ASSIGNMENT((#14666));
#14668=COLOUR_RGB('Grey',0.48,0.52,0.57);
#14669=FILL_AREA_STYLE_COLOUR('',#14668);
#14670=FILL_AREA_STYLE('',(#14669));
#14671=SURFACE_STYLE_FILL_AREA(#14670);
#14672=SURFACE_SIDE_STYLE('',(#14671));
#14673=SURFACE_STYLE_USAGE(.BOTH.,#14672);
#14674=PRESENTATION_STYLE_ASSIGNMENT((#14673));
#14675=COLOUR_RGB('Black',0.12,0.14,0.17);
#14676=FILL_AREA_STYLE_COLOUR('',#14675);
#14677=FILL_AREA_STYLE('',(#14676));
#14678=SURFACE_STYLE_FILL_AREA(#14677);
#14679=SURFACE_SIDE_STYLE('',(#14678));
#14680=SURFACE_STYLE_USAGE(.BOTH.,#14679);
#14681=PRESENTATION_STYLE_ASSIGNMENT((#14680));
#14682=COLOUR_RGB('Off White',0.89,0.88,0.83);
#14683=FILL_AREA_STYLE_COLOUR('',#14682);
#14684=FILL_AREA_STYLE('',(#14683));
#14685=SURFACE_STYLE_FILL_AREA(#14684);
#14686=SURFACE_SIDE_STYLE('',(#14685));
#14687=SURFACE_STYLE_USAGE(.BOTH.,#14686);
#14688=PRESENTATION_STYLE_ASSIGNMENT((#14687));
ENDSEC;
END-ISO-10303-21;
